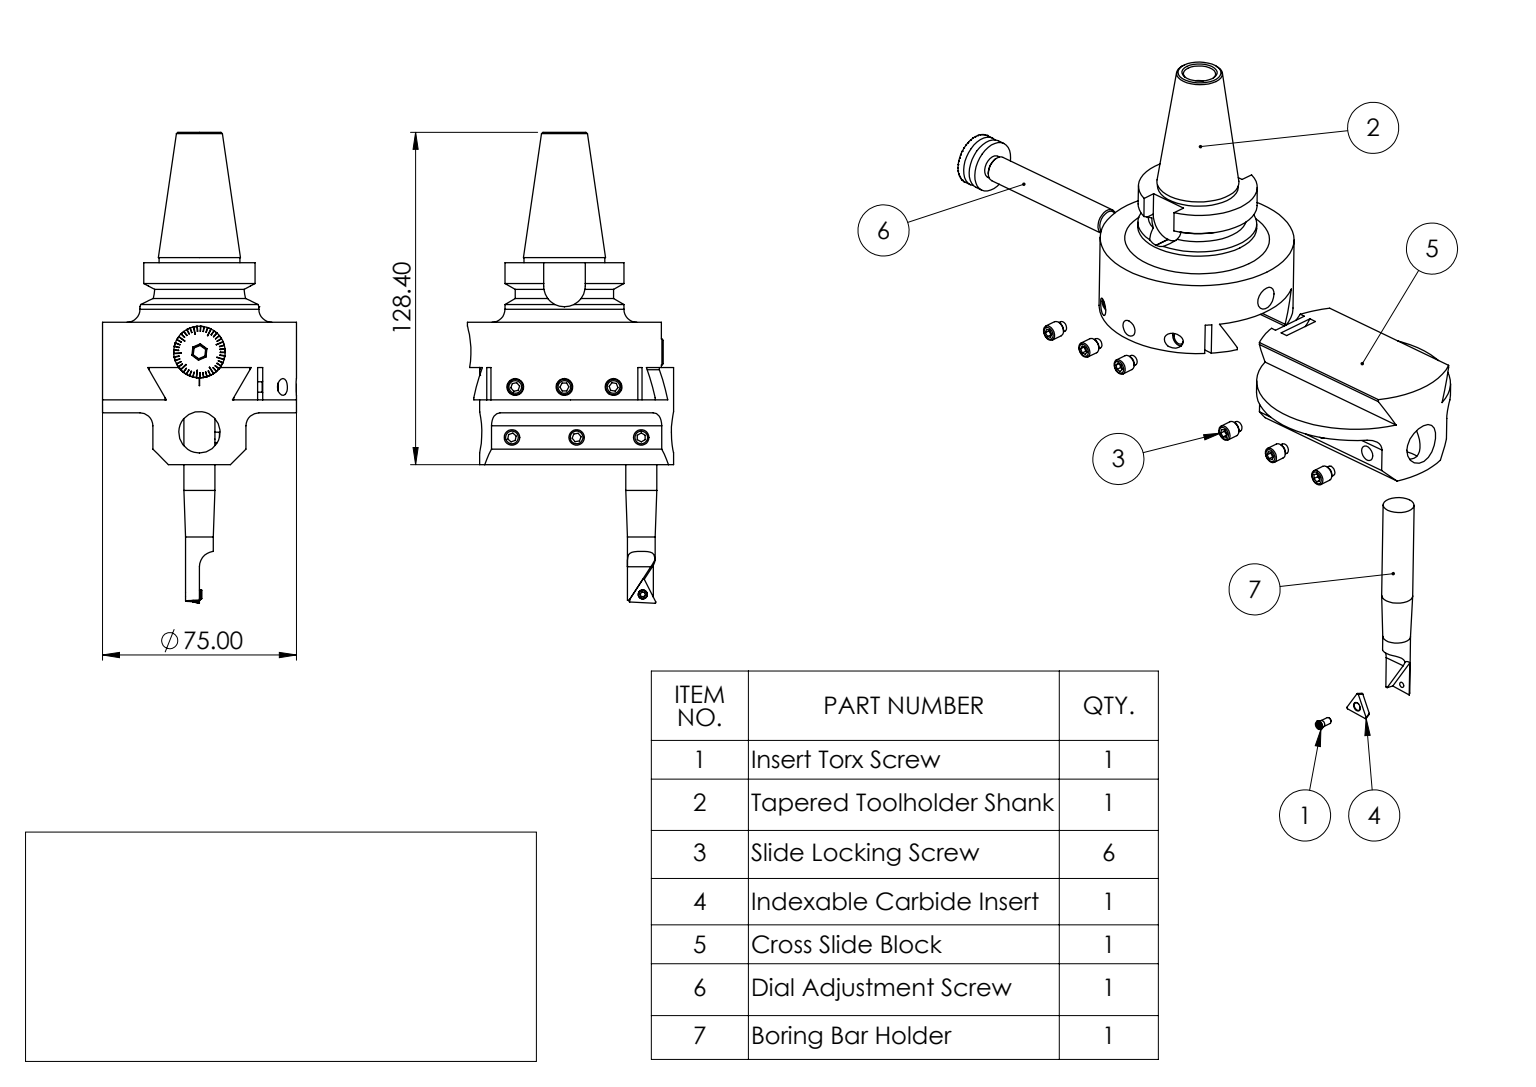
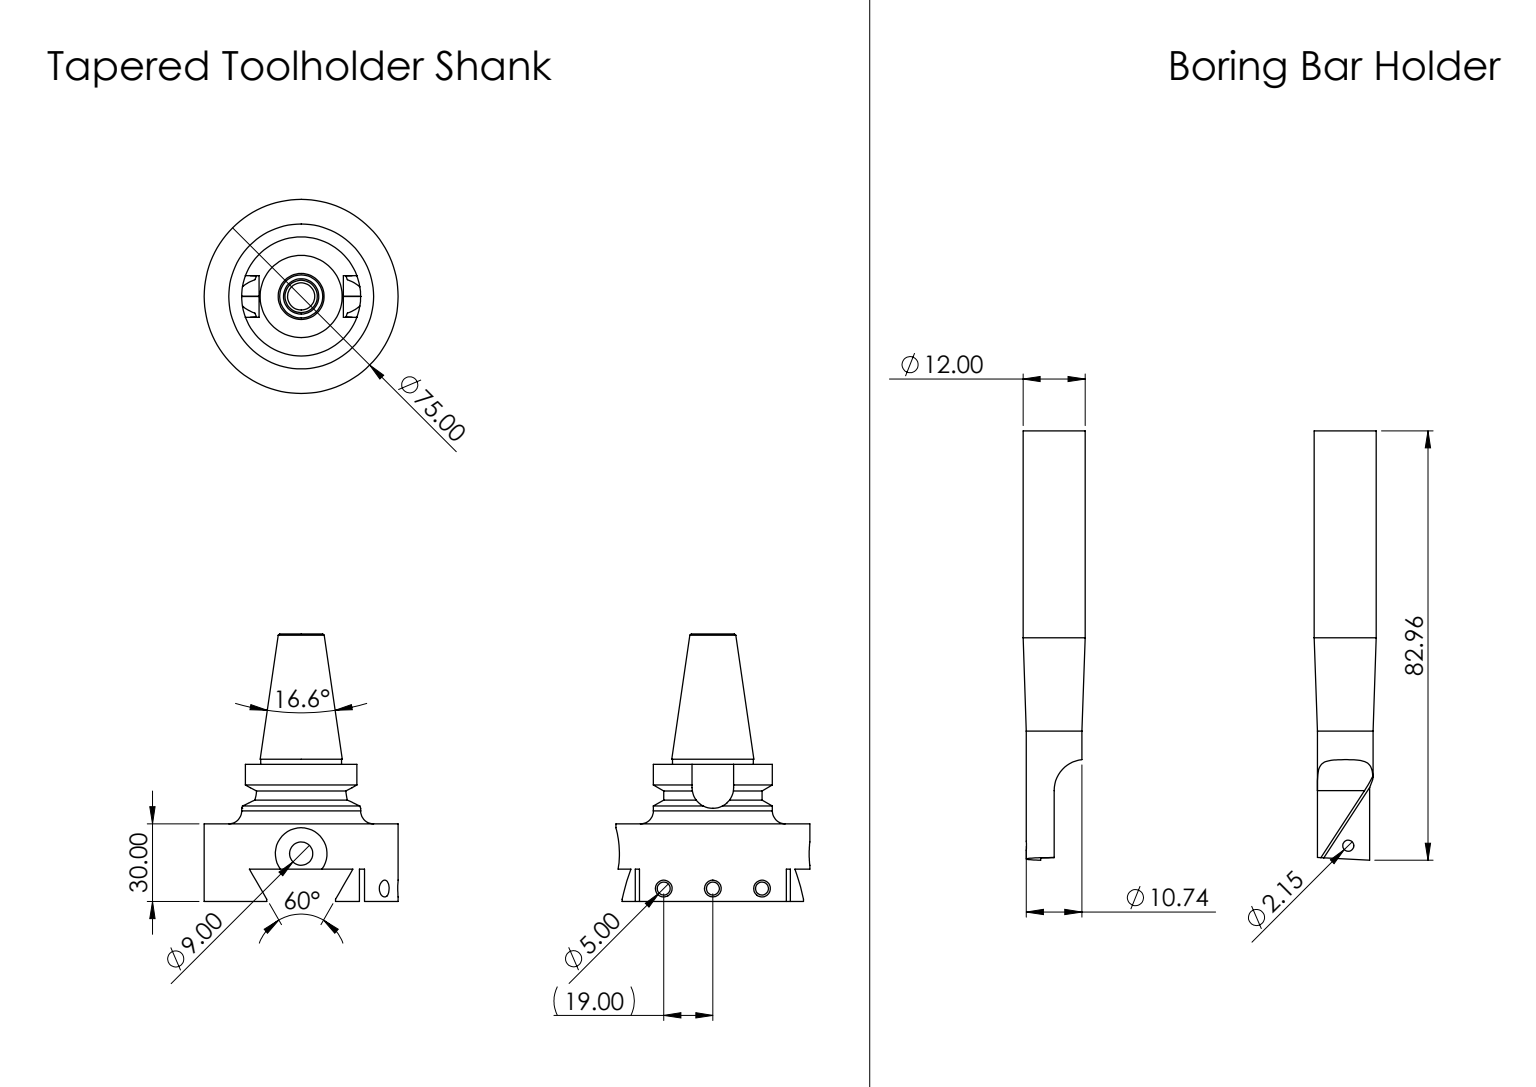
ISO-10303-21;
HEADER;
FILE_DESCRIPTION (('STEP AP214'),
    '1' );
FILE_NAME ('MAS-672',
    '2026-10-09T18:50:44',
    ( '' ),
    ( '' ),
    'SwSTEP 2.0',
    'SolidWorks 2026',
    '' );
FILE_SCHEMA (( 'AUTOMOTIVE_DESIGN' ));
ENDSEC;

DATA;
#1 = DIRECTION ( 'NONE',  ( 1.000000000000000000, 1.000000000000000078E-15, 0.000000000000000000 ) ) ;
#2 = ADVANCED_FACE ( 'NONE', ( #7489 ), #472, .F. ) ;
#3 = FACE_OUTER_BOUND ( 'NONE', #3774, .T. ) ;
#4 = EDGE_CURVE ( 'NONE', #9153, #8466, #14460, .T. ) ;
#5 =( BOUNDED_CURVE ( )  B_SPLINE_CURVE ( 3, ( #1335, #9589, #4703, #9365 ),
 .UNSPECIFIED., .F., .F. ) 
 B_SPLINE_CURVE_WITH_KNOTS ( ( 4, 4 ),
 ( 1.628044839356179940, 3.141592653589793116 ),
 .UNSPECIFIED. ) 
 CURVE ( )  GEOMETRIC_REPRESENTATION_ITEM ( )  RATIONAL_B_SPLINE_CURVE ( ( 1.000000000000000000, 0.8180365063541270576, 0.8180365063541270576, 1.000000000000000000 ) ) 
 REPRESENTATION_ITEM ( '' )  );
#6 = LINE ( 'NONE', #11551, #10906 ) ;
#7 = EDGE_CURVE ( 'NONE', #9450, #4202, #8492, .T. ) ;
#8 = LINE ( 'NONE', #14787, #7820 ) ;
#9 = CARTESIAN_POINT ( 'NONE',  ( -36.90121799483238618, -37.26927769664154511, 50.29562344872909563 ) ) ;
#10 = FACE_OUTER_BOUND ( 'NONE', #5268, .T. ) ;
#11 = ORIENTED_EDGE ( 'NONE', *, *, #1671, .F. ) ;
#12 = DIRECTION ( 'NONE',  ( 8.018662683283438208E-16, -5.975035461963189015E-16, -1.000000000000000000 ) ) ;
#13 = EDGE_LOOP ( 'NONE', ( #14568, #7332, #7097, #12565 ) ) ;
#15 = ORIENTED_EDGE ( 'NONE', *, *, #4138, .F. ) ;
#14 = CARTESIAN_POINT ( 'NONE',  ( -24.38380099443793725, -15.36048369738253427, 57.00231026484397745 ) ) ;
#16 = EDGE_CURVE ( 'NONE', #234, #9567, #717, .T. ) ;
#17 = VERTEX_POINT ( 'NONE', #8566 ) ;
#18 = AXIS2_PLACEMENT_3D ( 'NONE', #7899, #12589, #2105 ) ;
#19 = CYLINDRICAL_SURFACE ( 'NONE', #13148, 15.62500000000000000 ) ;
#20 = ORIENTED_EDGE ( 'NONE', *, *, #787, .F. ) ;
#21 = CYLINDRICAL_SURFACE ( 'NONE', #12948, 3.000000000000002665 ) ;
#22 = CARTESIAN_POINT ( 'NONE',  ( -15.49969986081095996, -67.00737899243799234, -5.497689735156000346 ) ) ;
#23 = CARTESIAN_POINT ( 'NONE',  ( 2.500300139188999182, -51.00737899243799944, -13.39525803434800011 ) ) ;
#24 = DIRECTION ( 'NONE',  ( 0.000000000000000000, 0.000000000000000000, 1.000000000000000000 ) ) ;
#25 = ADVANCED_FACE ( 'NONE', ( #12243 ), #13329, .T. ) ;
#26 = CARTESIAN_POINT ( 'NONE',  ( -19.99969986081099904, -13.50737899243800122, -13.01695671647154917 ) ) ;
#27 = CARTESIAN_POINT ( 'NONE',  ( -8.600581100527527667, -9.311215824554304632, 56.85231026484400019 ) ) ;
#28 = CARTESIAN_POINT ( 'NONE',  ( -21.52984724227062685, -49.79067269186487721, -17.51158402248789869 ) ) ;
#29 = ORIENTED_EDGE ( 'NONE', *, *, #1222, .T. ) ;
#30 = PLANE ( 'NONE',  #7847 ) ;
#31 = ORIENTED_EDGE ( 'NONE', *, *, #8737, .F. ) ;
#32 = DIRECTION ( 'NONE',  ( 0.4895147004624025855, -0.8719950447285834683, 9.135454576425998749E-16 ) ) ;
#33 = VERTEX_POINT ( 'NONE', #4056 ) ;
#34 = VERTEX_POINT ( 'NONE', #8713 ) ;
#35 = CARTESIAN_POINT ( 'NONE',  ( -10.39628701978575975, -6.002951807498697612, 56.85231026484398598 ) ) ;
#36 = VERTEX_POINT ( 'NONE', #13398 ) ;
#38 = EDGE_CURVE ( 'NONE', #4941, #11428, #1756, .T. ) ;
#37 = CARTESIAN_POINT ( 'NONE',  ( -15.57469986081333424, -23.50709773848279482, 57.00223526477140013 ) ) ;
#39 = CARTESIAN_POINT ( 'NONE',  ( -15.49969986081099904, 10.68321993080349763, 24.21206422150099868 ) ) ;
#40 = CARTESIAN_POINT ( 'NONE',  ( -10.66443468489866220, -90.61811337294874136, -7.838004541461820907 ) ) ;
#41 = CIRCLE ( 'NONE', #1011, 2.500000000000002220 ) ;
#42 = CARTESIAN_POINT ( 'NONE',  ( -7.506852801849951184, -44.86566843535796778, 21.38792573514972872 ) ) ;
#44 = CARTESIAN_POINT ( 'NONE',  ( -15.49969986081100615, -101.3912783891275069, -6.049618808461761255 ) ) ;
#43 = CARTESIAN_POINT ( 'NONE',  ( -15.50552586659557797, -13.55703840903364288, 56.85231026484398598 ) ) ;
#45 = ORIENTED_EDGE ( 'NONE', *, *, #9054, .F. ) ;
#46 = CARTESIAN_POINT ( 'NONE',  ( -15.17726793795939599, -10.75904990174046461, 51.00231026484399166 ) ) ;
#47 = CARTESIAN_POINT ( 'NONE',  ( -19.40475874296427250, -15.76281827183478512, -13.08441654828304657 ) ) ;
#48 = EDGE_LOOP ( 'NONE', ( #7800, #11011, #11564, #11938, #6650, #9579, #4015 ) ) ;
#49 = ORIENTED_EDGE ( 'NONE', *, *, #8035, .T. ) ;
#50 = CYLINDRICAL_SURFACE ( 'NONE', #2747, 15.62500000000000000 ) ;
#51 = FACE_BOUND ( 'NONE', #14476, .T. ) ;
#52 = ORIENTED_EDGE ( 'NONE', *, *, #5707, .T. ) ;
#53 = CARTESIAN_POINT ( 'NONE',  ( -10.22150846799388191, -38.48997916076172743, -17.62493476913342150 ) ) ;
#54 = EDGE_LOOP ( 'NONE', ( #11405, #3978, #7502, #8559 ) ) ;
#55 = EDGE_CURVE ( 'NONE', #11066, #9490, #2977, .T. ) ;
#56 = VECTOR ( 'NONE', #14424, 999.9999999999998863 ) ;
#57 = VECTOR ( 'NONE', #8652, 999.9999999999998863 ) ;
#58 = DIRECTION ( 'NONE',  ( -0.5104125104778984845, -0.8599296884906632021, 1.045284632676530333E-16 ) ) ;
#59 = CARTESIAN_POINT ( 'NONE',  ( -37.04494295528539993, 3.992621007561997892, 24.16206422150099442 ) ) ;
#60 = CARTESIAN_POINT ( 'NONE',  ( -15.49969986081091555, -109.7266455319748957, -5.512402352389309534 ) ) ;
#61 = CARTESIAN_POINT ( 'NONE',  ( -12.46042140754850713, -23.00808483377100444, 57.00231026484399166 ) ) ;
#62 = ORIENTED_EDGE ( 'NONE', *, *, #12874, .F. ) ;
#63 = DIRECTION ( 'NONE',  ( -0.3306575217771102193, 0.9437508163134058492, -8.290375725550400094E-16 ) ) ;
#64 = VECTOR ( 'NONE', #10695, 1000.000000000000000 ) ;
#65 = DIRECTION ( 'NONE',  ( 0.9354976265738682573, -0.3533329742249642913, 9.612616959383187437E-16 ) ) ;
#66 = ORIENTED_EDGE ( 'NONE', *, *, #12766, .T. ) ;
#67 = CIRCLE ( 'NONE', #8607, 9.974999999999999645 ) ;
#68 = AXIS2_PLACEMENT_3D ( 'NONE', #8168, #77, #12858 ) ;
#69 = CARTESIAN_POINT ( 'NONE',  ( -18.09969986081100402, -102.4362639876081289, -6.675878016713550522 ) ) ;
#70 = ORIENTED_EDGE ( 'NONE', *, *, #13189, .F. ) ;
#71 = DIRECTION ( 'NONE',  ( 0.000000000000000000, 0.000000000000000000, 1.000000000000000000 ) ) ;
#72 = EDGE_LOOP ( 'NONE', ( #9972, #5659, #4429, #2400 ) ) ;
#73 = EDGE_CURVE ( 'NONE', #9964, #7300, #12453, .T. ) ;
#74 = CARTESIAN_POINT ( 'NONE',  ( -5.499699860811000818, -46.50737899243799944, 22.50231026484399877 ) ) ;
#75 = DIRECTION ( 'NONE',  ( 1.000000000000000000, 0.000000000000000000, 0.000000000000000000 ) ) ;
#76 = ADVANCED_BREP_SHAPE_REPRESENTATION ( '', ( #2616, #6789 ), #5587 ) ;
#77 = DIRECTION ( 'NONE',  ( 0.7350174335289139105, -0.6780482080269579770, 9.945218953682734920E-16 ) ) ;
#78 = DIRECTION ( 'NONE',  ( 0.9931883319083343320, -0.1165201156931293391, 8.660254037844387408E-16 ) ) ;
#79 = AXIS2_PLACEMENT_3D ( 'NONE', #11806, #5987, #8360 ) ;
#80 = VECTOR ( 'NONE', #13700, 1000.000000000000114 ) ;
#81 = CARTESIAN_POINT ( 'NONE',  ( -15.49969986081099904, -32.00737899243799944, 24.21206422150100224 ) ) ;
#82 = FACE_OUTER_BOUND ( 'NONE', #1702, .T. ) ;
#83 = PLANE ( 'NONE',  #4186 ) ;
#84 = CARTESIAN_POINT ( 'NONE',  ( -7.424382730750140880, -13.52981220323889566, 56.85231026484400019 ) ) ;
#85 = ORIENTED_EDGE ( 'NONE', *, *, #97, .F. ) ;
#86 = CARTESIAN_POINT ( 'NONE',  ( -3.508527451664998686, -47.80641709811465745, -6.247689735156000346 ) ) ;
#87 = ORIENTED_EDGE ( 'NONE', *, *, #11967, .T. ) ;
#89 = EDGE_LOOP ( 'NONE', ( #13517, #1080, #433, #4734 ) ) ;
#88 = PLANE ( 'NONE',  #6660 ) ;
#90 = ORIENTED_EDGE ( 'NONE', *, *, #9916, .T. ) ;
#91 = CIRCLE ( 'NONE', #14500, 8.000000000000000000 ) ;
#92 = CIRCLE ( 'NONE', #3743, 3.249999999999999556 ) ;
#93 = EDGE_CURVE ( 'NONE', #6978, #3447, #6411, .T. ) ;
#94 = LINE ( 'NONE', #9566, #672 ) ;
#95 = ORIENTED_EDGE ( 'NONE', *, *, #10374, .T. ) ;
#96 = DIRECTION ( 'NONE',  ( -8.018662683283438208E-16, 5.975035461963189015E-16, 1.000000000000000000 ) ) ;
#97 = EDGE_CURVE ( 'NONE', #6821, #6890, #11166, .T. ) ;
#98 = CARTESIAN_POINT ( 'NONE',  ( -20.86490974387957209, -107.8289007898295182, -5.225852060212539563 ) ) ;
#99 =( BOUNDED_CURVE ( )  B_SPLINE_CURVE ( 3, ( #13212, #2486, #10670, #275 ),
 .UNSPECIFIED., .F., .T. ) 
 B_SPLINE_CURVE_WITH_KNOTS ( ( 4, 4 ),
 ( 4.712388980384689674, 6.283185307179586232 ),
 .UNSPECIFIED. ) 
 CURVE ( )  GEOMETRIC_REPRESENTATION_ITEM ( )  RATIONAL_B_SPLINE_CURVE ( ( 1.000000000000000000, 0.8047378541243649375, 0.8047378541243649375, 1.000000000000000000 ) ) 
 REPRESENTATION_ITEM ( '' )  );
#100 = LINE ( 'NONE', #14015, #4170 ) ;
#101 = CARTESIAN_POINT ( 'NONE',  ( 0.000000000000000000, 0.000000000000000000, 0.000000000000000000 ) ) ;
#102 = EDGE_CURVE ( 'NONE', #7782, #14676, #12670, .T. ) ;
#103 = DIRECTION ( 'NONE',  ( -0.9320450512859426162, -0.3618458327180910095, 0.01896353653557692268 ) ) ;
#104 = AXIS2_PLACEMENT_3D ( 'NONE', #5495, #8007, #12779 ) ;
#105 = CARTESIAN_POINT ( 'NONE',  ( -11.67714598312096008, -19.46131314156662384, 56.85231026484400019 ) ) ;
#106 = CARTESIAN_POINT ( 'NONE',  ( -5.499699860810999041, -13.50737899243800122, 6.712064221500998684 ) ) ;
#107 = APPLICATION_CONTEXT ( 'automotive_design' ) ;
#108 = ORIENTED_EDGE ( 'NONE', *, *, #1414, .F. ) ;
#109 = CARTESIAN_POINT ( 'NONE',  ( -14.90757383352018195, -17.97794807782672777, -13.28437183209255146 ) ) ;
#110 = ORIENTED_EDGE ( 'NONE', *, *, #5500, .T. ) ;
#111 = AXIS2_PLACEMENT_3D ( 'NONE', #10208, #14881, #11508 ) ;
#112 = ORIENTED_EDGE ( 'NONE', *, *, #3083, .T. ) ;
#113 = ORIENTED_EDGE ( 'NONE', *, *, #12612, .F. ) ;
#114 = CARTESIAN_POINT ( 'NONE',  ( -9.989347722329675605, -44.50737899243799944, -5.497689735156000346 ) ) ;
#115 = EDGE_CURVE ( 'NONE', #11608, #7250, #12699, .T. ) ;
#116 = CARTESIAN_POINT ( 'NONE',  ( 4.650967236384746073, -37.88568168827513460, 51.12989147907354948 ) ) ;
#117 = EDGE_CURVE ( 'NONE', #4448, #10428, #688, .T. ) ;
#118 = VERTEX_POINT ( 'NONE', #5499 ) ;
#119 = CARTESIAN_POINT ( 'NONE',  ( -15.49969986081092088, -13.50737899243822504, 57.00231026484397745 ) ) ;
#120 = LINE ( 'NONE', #11886, #1708 ) ;
#121 = CARTESIAN_POINT ( 'NONE',  ( -1.821162622431182765, -43.50737899243799234, -5.497689735156000346 ) ) ;
#122 = AXIS2_PLACEMENT_3D ( 'NONE', #7053, #14187, #10744 ) ;
#123 = LINE ( 'NONE', #4934, #14525 ) ;
#124 = COLOUR_RGB ( '', 0.72549020, 0.75294118, 0.79215686) ;
#126 = LINE ( 'NONE', #11658, #7291 ) ;
#125 = CARTESIAN_POINT ( 'NONE',  ( -7.500433020662222283, -49.00523987278725713, -5.609464624471996785 ) ) ;
#127 = ORIENTED_EDGE ( 'NONE', *, *, #115, .F. ) ;
#128 = DIRECTION ( 'NONE',  ( 0.000000000000000000, 0.000000000000000000, -1.000000000000000000 ) ) ;
#129 = DIRECTION ( 'NONE',  ( 0.9645173894937585368, 0.2640193276336892936, 6.156614753256587028E-16 ) ) ;
#130 = ORIENTED_EDGE ( 'NONE', *, *, #8611, .T. ) ;
#131 = CARTESIAN_POINT ( 'NONE',  ( -8.744347237509680681, -17.93190845158491342, 57.00231026484399166 ) ) ;
#132 = ADVANCED_FACE ( 'NONE', ( #4206 ), #14685, .F. ) ;
#133 = EDGE_LOOP ( 'NONE', ( #10977, #6757, #1819, #5580 ) ) ;
#134 = CARTESIAN_POINT ( 'NONE',  ( -3.508527451664998686, -47.37340439622244048, -6.997689735156000346 ) ) ;
#135 = ORIENTED_EDGE ( 'NONE', *, *, #11324, .F. ) ;
#136 = EDGE_CURVE ( 'NONE', #14079, #280, #5835, .T. ) ;
#137 = VECTOR ( 'NONE', #5946, 999.9999999999998863 ) ;
#138 = CARTESIAN_POINT ( 'NONE',  ( 7.500245791298697284, 3.992621007561997892, 24.26206422150100295 ) ) ;
#139 = DIRECTION ( 'NONE',  ( 0.000000000000000000, 0.1872998510044759646, 0.9823027872370621028 ) ) ;
#140 = ADVANCED_FACE ( 'NONE', ( #4434 ), #1914, .T. ) ;
#141 = DIRECTION ( 'NONE',  ( -8.018662683283438208E-16, 5.975035461963189015E-16, 1.000000000000000000 ) ) ;
#142 = CARTESIAN_POINT ( 'NONE',  ( 18.53245405280430802, -27.00737899243800300, 8.462064221501000461 ) ) ;
#143 = ORIENTED_EDGE ( 'NONE', *, *, #1430, .T. ) ;
#144 = FACE_OUTER_BOUND ( 'NONE', #9192, .T. ) ;
#145 = DIRECTION ( 'NONE',  ( 8.660254037844386422E-16, -0.8660254037844387076, -0.4999999999999998890 ) ) ;
#146 = ORIENTED_EDGE ( 'NONE', *, *, #10088, .T. ) ;
#147 = DIRECTION ( 'NONE',  ( -1.000000000000000000, 1.499759782661860071E-32, -1.224646799147350002E-16 ) ) ;
#148 = EDGE_LOOP ( 'NONE', ( #12283, #12107, #2323, #5497, #12543, #7117, #9032, #3787, #13140, #10913, #13822, #11755, #4698, #10634, #4086, #13650, #1565 ) ) ;
#149 = PLANE ( 'NONE',  #14987 ) ;
#150 = VERTEX_POINT ( 'NONE', #916 ) ;
#151 = CARTESIAN_POINT ( 'NONE',  ( 2.500300139188999182, -51.00737899243799944, -13.39525803434800011 ) ) ;
#152 = CARTESIAN_POINT ( 'NONE',  ( -1.821162622431182765, -43.50737899243799234, -5.497689735156000346 ) ) ;
#153 = CARTESIAN_POINT ( 'NONE',  ( -28.28282149594069850, -32.00737899243799944, -17.99768973515599768 ) ) ;
#154 = FACE_OUTER_BOUND ( 'NONE', #467, .T. ) ;
#155 = DIRECTION ( 'NONE',  ( 0.000000000000000000, 0.000000000000000000, 1.000000000000000000 ) ) ;
#156 = CARTESIAN_POINT ( 'NONE',  ( -17.71860670988920816, -11.85398021090886367, 51.00231026484399166 ) ) ;
#157 = VECTOR ( 'NONE', #7597, 1000.000000000000114 ) ;
#158 = VECTOR ( 'NONE', #4649, 1000.000000000000000 ) ;
#159 = EDGE_CURVE ( 'NONE', #10747, #3108, #3053, .T. ) ;
#160 = CARTESIAN_POINT ( 'NONE',  ( -20.87112600995946110, -106.2635794615412834, -5.497689735156005675 ) ) ;
#161 = ORIENTED_EDGE ( 'NONE', *, *, #9054, .T. ) ;
#162 = LINE ( 'NONE', #9710, #2630 ) ;
#163 = CARTESIAN_POINT ( 'NONE',  ( -37.26807582031575805, -37.15669500878452425, 50.03818627108570638 ) ) ;
#164 = DIRECTION ( 'NONE',  ( 0.000000000000000000, 1.131341397376178572E-16, -1.000000000000000000 ) ) ;
#165 = ORIENTED_EDGE ( 'NONE', *, *, #2149, .T. ) ;
#166 = DIRECTION ( 'NONE',  ( 8.018662683283438208E-16, -5.975035461963189015E-16, -1.000000000000000000 ) ) ;
#167 = ORIENTED_EDGE ( 'NONE', *, *, #12641, .F. ) ;
#169 = ORIENTED_EDGE ( 'NONE', *, *, #13036, .F. ) ;
#168 = FACE_BOUND ( 'NONE', #682, .T. ) ;
#170 = ORIENTED_EDGE ( 'NONE', *, *, #333, .F. ) ;
#171 = CARTESIAN_POINT ( 'NONE',  ( -15.49969986081092088, -13.50737899243822504, 56.85231026484398598 ) ) ;
#172 = ORIENTED_EDGE ( 'NONE', *, *, #3900, .F. ) ;
#173 = FACE_OUTER_BOUND ( 'NONE', #4854, .T. ) ;
#174 = CARTESIAN_POINT ( 'NONE',  ( -15.49969986081099904, -44.50737899243799944, -109.5506571639849938 ) ) ;
#175 = SHAPE_REPRESENTATION_RELATIONSHIP ( 'NONE' , 'NONE' ,  #13495, #6601 ) ;
#176 = CARTESIAN_POINT ( 'NONE',  ( -18.41596830400278506, -14.76384693893611910, 57.00231026484397745 ) ) ;
#177 = EDGE_CURVE ( 'NONE', #13055, #12587, #8525, .T. ) ;
#178 = AXIS2_PLACEMENT_3D ( 'NONE', #14596, #7550, #6095 ) ;
#179 = CARTESIAN_POINT ( 'NONE',  ( -15.49969986081099371, -9.007378992438001220, -13.28793577849899599 ) ) ;
#180 = CARTESIAN_POINT ( 'NONE',  ( -28.78282149594069850, -32.00737899243799944, 24.21206422150099868 ) ) ;
#181 = EDGE_CURVE ( 'NONE', #13469, #7197, #14834, .T. ) ;
#182 = CARTESIAN_POINT ( 'NONE',  ( 4.224496369445544630, -38.22985747236960918, -12.39136299437819488 ) ) ;
#183 = EDGE_LOOP ( 'NONE', ( #8383, #10689, #169, #12159 ) ) ;
#184 = ORIENTED_EDGE ( 'NONE', *, *, #9513, .F. ) ;
#185 = AXIS2_PLACEMENT_3D ( 'NONE', #4466, #10423, #5753 ) ;
#186 = VERTEX_POINT ( 'NONE', #14912 ) ;
#187 = CARTESIAN_POINT ( 'NONE',  ( 2.883830742001312508, -40.08477038827061989, 52.18712618527332125 ) ) ;
#188 = ORIENTED_EDGE ( 'NONE', *, *, #5314, .T. ) ;
#189 = CIRCLE ( 'NONE', #12147, 2.499999999999999556 ) ;
#190 = DIRECTION ( 'NONE',  ( 1.000000000000000000, 1.000000000000000078E-15, 1.000000000000000078E-15 ) ) ;
#191 = FACE_OUTER_BOUND ( 'NONE', #10169, .T. ) ;
#192 = DIRECTION ( 'NONE',  ( 0.5975035461963189576, 0.8018662683283437342, 0.000000000000000000 ) ) ;
#193 = EDGE_CURVE ( 'NONE', #1606, #4275, #8746, .T. ) ;
#194 = EDGE_CURVE ( 'NONE', #4315, #8561, #7264, .T. ) ;
#195 = CARTESIAN_POINT ( 'NONE',  ( -15.49969986081091022, -13.50737899243823215, 46.00231026484398456 ) ) ;
#197 = CARTESIAN_POINT ( 'NONE',  ( -8.681233859935401753, -6.226640953275941470, 56.85231026484398598 ) ) ;
#196 = LINE ( 'NONE', #3708, #2723 ) ;
#198 = EDGE_CURVE ( 'NONE', #14370, #12333, #7164, .T. ) ;
#199 = EDGE_LOOP ( 'NONE', ( #11824, #6464, #11368, #3598 ) ) ;
#200 = CARTESIAN_POINT ( 'NONE',  ( -15.49969986081099904, -19.50737899243800300, 24.21206422150100224 ) ) ;
#201 = AXIS2_PLACEMENT_3D ( 'NONE', #9207, #12513, #13890 ) ;
#202 = CARTESIAN_POINT ( 'NONE',  ( -7.499699860810999041, -19.50737899243799589, 51.00231026484400587 ) ) ;
#203 = EDGE_LOOP ( 'NONE', ( #1328, #2305, #6910, #14868 ) ) ;
#204 = ORIENTED_EDGE ( 'NONE', *, *, #10815, .T. ) ;
#205 = AXIS2_PLACEMENT_3D ( 'NONE', #2653, #1576, #13144 ) ;
#206 = CARTESIAN_POINT ( 'NONE',  ( -16.55248250669792753, -52.45523696625489407, 56.99108552064786437 ) ) ;
#207 = ORIENTED_EDGE ( 'NONE', *, *, #11956, .F. ) ;
#208 =( NAMED_UNIT ( * ) SI_UNIT ( $, .STERADIAN. ) SOLID_ANGLE_UNIT ( ) );
#209 = CARTESIAN_POINT ( 'NONE',  ( 7.464989229556169725, 4.086072560925113173, 25.52420958079008884 ) ) ;
#210 = CARTESIAN_POINT ( 'NONE',  ( -17.47506273705024071, -21.33739760717825718, 56.85231026484400019 ) ) ;
#211 = EDGE_CURVE ( 'NONE', #12427, #2827, #11544, .T. ) ;
#212 = DIRECTION ( 'NONE',  ( 0.6859287159822015090, -0.7276687409742212953, 9.848077530122081084E-16 ) ) ;
#213 = CARTESIAN_POINT ( 'NONE',  ( -15.49969986081099016, -52.50737899243799944, 27.50231026484399521 ) ) ;
#214 = EDGE_CURVE ( 'NONE', #2810, #1679, #14130, .T. ) ;
#215 = ORIENTED_EDGE ( 'NONE', *, *, #13065, .F. ) ;
#216 = DIRECTION ( 'NONE',  ( 0.000000000000000000, 0.000000000000000000, 1.000000000000000000 ) ) ;
#217 = CARTESIAN_POINT ( 'NONE',  ( -10.84210729886283531, -6.910555398701176522, 56.85231026484398598 ) ) ;
#218 = ORIENTED_EDGE ( 'NONE', *, *, #1842, .T. ) ;
#219 = PLANE ( 'NONE',  #12030 ) ;
#220 = CARTESIAN_POINT ( 'NONE',  ( -15.49969986081099904, 0.9926210075619987805, 24.21206422150099868 ) ) ;
#221 = VERTEX_POINT ( 'NONE', #11762 ) ;
#222 = VECTOR ( 'NONE', #14585, 1000.000000000000000 ) ;
#223 = DIRECTION ( 'NONE',  ( -1.000000000000000000, -1.201369187114119994E-15, -9.616040805000176517E-16 ) ) ;
#224 = ORIENTED_EDGE ( 'NONE', *, *, #12134, .T. ) ;
#225 = FACE_OUTER_BOUND ( 'NONE', #3388, .T. ) ;
#226 = CARTESIAN_POINT ( 'NONE',  ( -15.49969986081098838, -17.75737899243799944, 48.00231026484399877 ) ) ;
#227 = EDGE_CURVE ( 'NONE', #9086, #8293, #11691, .T. ) ;
#228 = LINE ( 'NONE', #8628, #3240 ) ;
#230 = VECTOR ( 'NONE', #6999, 1000.000000000000000 ) ;
#229 = CARTESIAN_POINT ( 'NONE',  ( -7.753733168396170328, -46.50737899243799944, 47.00231026484399877 ) ) ;
#231 = AXIS2_PLACEMENT_3D ( 'NONE', #5849, #3193, #3340 ) ;
#232 = PLANE ( 'NONE',  #13853 ) ;
#233 = DIRECTION ( 'NONE',  ( 0.000000000000000000, 0.000000000000000000, 1.000000000000000000 ) ) ;
#234 = VERTEX_POINT ( 'NONE', #10472 ) ;
#235 = DIRECTION ( 'NONE',  ( -8.018662683283438208E-16, 5.975035461963189015E-16, 1.000000000000000000 ) ) ;
#236 = CARTESIAN_POINT ( 'NONE',  ( -16.32407967933980686, -20.53418644068968746, 57.00231026484399166 ) ) ;
#237 = CARTESIAN_POINT ( 'NONE',  ( -15.49969986081099727, -52.50737899243799944, 2.502310264843994769 ) ) ;
#238 = ORIENTED_EDGE ( 'NONE', *, *, #5431, .T. ) ;
#239 = DIRECTION ( 'NONE',  ( 8.018662683283438208E-16, -5.975035461963189015E-16, -1.000000000000000000 ) ) ;
#240 = VECTOR ( 'NONE', #12413, 1000.000000000000000 ) ;
#241 = ORIENTED_EDGE ( 'NONE', *, *, #492, .T. ) ;
#243 = ORIENTED_EDGE ( 'NONE', *, *, #13545, .T. ) ;
#242 = CARTESIAN_POINT ( 'NONE',  ( -18.04596724311489808, -11.61005040962811563, 57.00231026484397745 ) ) ;
#244 = ORIENTED_EDGE ( 'NONE', *, *, #12022, .T. ) ;
#245 = AXIS2_PLACEMENT_3D ( 'NONE', #11135, #508, #11280 ) ;
#246 = DIRECTION ( 'NONE',  ( 0.6626200482157384997, -0.03919731383111437623, -0.7479293030032968526 ) ) ;
#247 = ORIENTED_EDGE ( 'NONE', *, *, #4682, .F. ) ;
#248 = EDGE_CURVE ( 'NONE', #9045, #3429, #2887, .T. ) ;
#249 = PLANE ( 'NONE',  #11119 ) ;
#250 = CYLINDRICAL_SURFACE ( 'NONE', #2706, 6.000000000000000000 ) ;
#251 = CARTESIAN_POINT ( 'NONE',  ( 4.510281037539698445E-14, -66.39050128843828702, 86.90304541097793845 ) ) ;
#252 = DIRECTION ( 'NONE',  ( 0.5975035461963189576, 0.8018662683283437342, 0.000000000000000000 ) ) ;
#253 = CIRCLE ( 'NONE', #14173, 37.50000000000000000 ) ;
#254 = CARTESIAN_POINT ( 'NONE',  ( -24.01584079503567182, -10.37104457333969876, 57.00231026484397745 ) ) ;
#255 = CARTESIAN_POINT ( 'NONE',  ( -15.47224238247604511, -13.54916519690201149, 56.85231026484398598 ) ) ;
#256 = VECTOR ( 'NONE', #11415, 1000.000000000000114 ) ;
#257 = ORIENTED_EDGE ( 'NONE', *, *, #6613, .T. ) ;
#258 = SURFACE_SIDE_STYLE ('',( #7350 ) ) ;
#259 = VERTEX_POINT ( 'NONE', #1213 ) ;
#260 = ORIENTED_EDGE ( 'NONE', *, *, #6343, .T. ) ;
#261 = CARTESIAN_POINT ( 'NONE',  ( 5.515696375138871232, -37.41693849659856141, 50.56059116161328859 ) ) ;
#262 = ORIENTED_EDGE ( 'NONE', *, *, #3647, .F. ) ;
#263 = CARTESIAN_POINT ( 'NONE',  ( -23.39388780995641781, -11.80648316271623877, 56.85231026484398598 ) ) ;
#264 = PRODUCT ( 'Boring Bar Holder', 'Boring Bar Holder', '', ( #2047 ) ) ;
#265 = DIRECTION ( 'NONE',  ( 0.000000000000000000, 0.000000000000000000, 1.000000000000000000 ) ) ;
#266 = EDGE_CURVE ( 'NONE', #5839, #14925, #4584, .T. ) ;
#267 = EDGE_CURVE ( 'NONE', #7737, #2967, #4813, .T. ) ;
#268 = DIRECTION ( 'NONE',  ( 0.000000000000000000, 1.224646799147350002E-16, -1.000000000000000000 ) ) ;
#269 = CARTESIAN_POINT ( 'NONE',  ( -11.86438417805047862, -90.99861266563027584, -9.452020815084084759 ) ) ;
#270 = CIRCLE ( 'NONE', #3683, 9.974999999999999645 ) ;
#271 = DIRECTION ( 'NONE',  ( 1.000000000000000000, -3.922012711866029438E-32, 3.202566417187950042E-16 ) ) ;
#273 = CARTESIAN_POINT ( 'NONE',  ( -34.99969986081099904, -19.50737899243800300, 51.53354502093799994 ) ) ;
#272 = CARTESIAN_POINT ( 'NONE',  ( -7.749729581313432369, -48.02091033734640035, -3.487279356396127739 ) ) ;
#274 = EDGE_LOOP ( 'NONE', ( #8027, #11892 ) ) ;
#275 = CARTESIAN_POINT ( 'NONE',  ( -15.49969986081099727, -36.50737899243799944, 2.502310264843996546 ) ) ;
#276 = VERTEX_POINT ( 'NONE', #1064 ) ;
#277 = ORIENTED_EDGE ( 'NONE', *, *, #6216, .F. ) ;
#278 = CARTESIAN_POINT ( 'NONE',  ( 21.96528021387864271, -29.82714745920393185, 22.58218370277269571 ) ) ;
#279 = CARTESIAN_POINT ( 'NONE',  ( -5.499699860811003482, -46.50737899243799944, 44.50231026484399877 ) ) ;
#280 = VERTEX_POINT ( 'NONE', #11617 ) ;
#281 = CARTESIAN_POINT ( 'NONE',  ( -14.45170227088251202, -36.55910949265851428, -17.98655532003696678 ) ) ;
#282 = EDGE_CURVE ( 'NONE', #626, #3416, #13005, .T. ) ;
#283 = EDGE_CURVE ( 'NONE', #10750, #11940, #6056, .T. ) ;
#284 = ADVANCED_FACE ( 'NONE', ( #2513 ), #11846, .F. ) ;
#285 = DIRECTION ( 'NONE',  ( 0.000000000000000000, 0.000000000000000000, -1.000000000000000000 ) ) ;
#286 = AXIS2_PLACEMENT_3D ( 'NONE', #4236, #8813, #2856 ) ;
#287 = CARTESIAN_POINT ( 'NONE',  ( -15.49969986081099904, -32.00737899243799944, 24.21206422150100224 ) ) ;
#288 = EDGE_CURVE ( 'NONE', #14042, #11463, #13916, .T. ) ;
#289 = CARTESIAN_POINT ( 'NONE',  ( -24.32830346761242879, -18.15026423267100597, 56.85231026484398598 ) ) ;
#290 = PLANE ( 'NONE',  #9367 ) ;
#291 = ORIENTED_EDGE ( 'NONE', *, *, #2351, .F. ) ;
#292 = CARTESIAN_POINT ( 'NONE',  ( 4.500300139189000959, -19.50737899243801010, 55.93350807262470425 ) ) ;
#293 = CARTESIAN_POINT ( 'NONE',  ( 0.8003001391889992266, 11.99262100756199878, 24.26206422150100295 ) ) ;
#294 = ORIENTED_EDGE ( 'NONE', *, *, #11168, .F. ) ;
#295 = DIRECTION ( 'NONE',  ( 0.9437508163134050720, 0.3306575217771122732, 5.591929034707472732E-16 ) ) ;
#296 = DIRECTION ( 'NONE',  ( 0.000000000000000000, 1.000000000000000000, 1.224646799147350002E-16 ) ) ;
#297 = ORIENTED_EDGE ( 'NONE', *, *, #1602, .F. ) ;
#298 = LINE ( 'NONE', #4183, #349 ) ;
#299 = ORIENTED_EDGE ( 'NONE', *, *, #12335, .F. ) ;
#300 = DIRECTION ( 'NONE',  ( 1.000000000000000000, 1.201369187114119994E-15, 9.616040805000176517E-16 ) ) ;
#301 = VECTOR ( 'NONE', #1890, 1000.000000000000000 ) ;
#302 = EDGE_CURVE ( 'NONE', #14153, #6582, #13638, .T. ) ;
#303 = EDGE_CURVE ( 'NONE', #11878, #6778, #8167, .T. ) ;
#304 = CARTESIAN_POINT ( 'NONE',  ( -15.49969986081100437, -101.4268716156739600, -6.728778029351857981 ) ) ;
#305 = DIRECTION ( 'NONE',  ( -8.673617379884027583E-16, 1.000000000000000000, 0.000000000000000000 ) ) ;
#306 = DIRECTION ( 'NONE',  ( 0.2301973227387160703, -0.9731439732146149879, 7.660444431189776467E-16 ) ) ;
#307 = VECTOR ( 'NONE', #2927, 999.9999999999998863 ) ;
#308 = CIRCLE ( 'NONE', #8106, 9.974999999999999645 ) ;
#309 = VECTOR ( 'NONE', #4436, 1000.000000000000000 ) ;
#310 = LINE ( 'NONE', #9632, #1371 ) ;
#311 = ORIENTED_EDGE ( 'NONE', *, *, #9034, .F. ) ;
#312 = DIRECTION ( 'NONE',  ( 1.000000000000000000, -3.922012711866029438E-32, 3.202566417187950042E-16 ) ) ;
#313 = DIRECTION ( 'NONE',  ( 1.000000000000000000, 1.201369187114119994E-15, 9.616040805000176517E-16 ) ) ;
#314 = ADVANCED_FACE ( 'NONE', ( #7004, #5865, #10542, #6834 ), #10286, .F. ) ;
#315 = CARTESIAN_POINT ( 'NONE',  ( -23.54151295824578227, -12.77219731018227300, 57.00231026484397745 ) ) ;
#316 = CARTESIAN_POINT ( 'NONE',  ( -6.938526287600617515, -8.388108336439909607, 57.00231026484399166 ) ) ;
#318 = ORIENTED_EDGE ( 'NONE', *, *, #7751, .T. ) ;
#317 = CARTESIAN_POINT ( 'NONE',  ( -14.61203582816999891, -107.9994814593942607, -7.057848339359947154 ) ) ;
#319 = ORIENTED_EDGE ( 'NONE', *, *, #11952, .F. ) ;
#320 = DIRECTION ( 'NONE',  ( -0.1855175943453192255, -0.9826409426582660700, 4.383711467890751032E-16 ) ) ;
#321 = FACE_OUTER_BOUND ( 'NONE', #7198, .T. ) ;
#322 = EDGE_LOOP ( 'NONE', ( #14404, #10872, #12403, #8371 ) ) ;
#323 = VECTOR ( 'NONE', #13122, 1000.000000000000114 ) ;
#324 =( BOUNDED_CURVE ( )  B_SPLINE_CURVE ( 3, ( #292, #8307, #2730, #6008 ),
 .UNSPECIFIED., .F., .T. ) 
 B_SPLINE_CURVE_WITH_KNOTS ( ( 4, 4 ),
 ( 1.008260082251040135, 1.208720131788790120 ),
 .UNSPECIFIED. ) 
 CURVE ( )  GEOMETRIC_REPRESENTATION_ITEM ( )  RATIONAL_B_SPLINE_CURVE ( ( 1.000000000000000000, 0.9966541165307394312, 0.9966541165307394312, 1.000000000000000000 ) ) 
 REPRESENTATION_ITEM ( '' )  );
#325 = DIRECTION ( 'NONE',  ( 0.9988970074402866439, -0.04695496274985035134, 8.290375725550441510E-16 ) ) ;
#326 = VECTOR ( 'NONE', #4845, 1000.000000000000000 ) ;
#327 = ADVANCED_FACE ( 'NONE', ( #7907 ), #7823, .T. ) ;
#328 = PLANE ( 'NONE',  #5014 ) ;
#329 = DIRECTION ( 'NONE',  ( -8.018662683283438208E-16, 5.975035461963189015E-16, 1.000000000000000000 ) ) ;
#330 = CARTESIAN_POINT ( 'NONE',  ( 0.000000000000000000, 0.000000000000000000, 0.000000000000000000 ) ) ;
#331 = CARTESIAN_POINT ( 'NONE',  ( -16.66466864975539153, -9.150908980254410352, -13.27094003038157943 ) ) ;
#332 = B_SPLINE_CURVE_WITH_KNOTS ( 'NONE', 3,
 ( #3786, #14269, #2413, #7056, #11734, #2637, #7211, #5838 ),
 .UNSPECIFIED., .F., .F.,
 ( 4, 2, 2, 4 ),
 ( 0.000000000000000000, 0.2500000000000007216, 0.5000000000000014433, 1.000000000000000000 ),
 .UNSPECIFIED. ) ;
#333 = EDGE_CURVE ( 'NONE', #11915, #14532, #10956, .T. ) ;
#334 = EDGE_CURVE ( 'NONE', #9332, #3237, #5095, .T. ) ;
#335 = AXIS2_PLACEMENT_3D ( 'NONE', #317, #9563, #3755 ) ;
#336 = DIRECTION ( 'NONE',  ( 8.018662683283438208E-16, -5.975035461963189015E-16, -1.000000000000000000 ) ) ;
#337 = VERTEX_POINT ( 'NONE', #13812 ) ;
#338 = CARTESIAN_POINT ( 'NONE',  ( -15.49969986081099904, -57.00737899243801365, 57.00231026484399166 ) ) ;
#339 = CONICAL_SURFACE ( 'NONE', #2284, 1664.279482350500075, 1.029744258676650093 ) ;
#340 = ORIENTED_EDGE ( 'NONE', *, *, #454, .F. ) ;
#341 = LINE ( 'NONE', #7503, #3156 ) ;
#342 = DIRECTION ( 'NONE',  ( -1.169602638241521591E-15, 0.1872998510044552312, 0.9823027872370662106 ) ) ;
#343 = ORIENTED_EDGE ( 'NONE', *, *, #4783, .T. ) ;
#344 = ORIENTED_EDGE ( 'NONE', *, *, #5377, .F. ) ;
#345 = CARTESIAN_POINT ( 'NONE',  ( -15.49969986081099904, -32.00737899243799944, 24.21206422150100224 ) ) ;
#346 = ORIENTED_EDGE ( 'NONE', *, *, #6966, .T. ) ;
#347 = LINE ( 'NONE', #11884, #5404 ) ;
#348 = DIRECTION ( 'NONE',  ( 8.018662683283438208E-16, -5.975035461963189015E-16, -1.000000000000000000 ) ) ;
#349 = VECTOR ( 'NONE', #8838, 1000.000000000000114 ) ;
#350 = FILL_AREA_STYLE ('',( #10818 ) ) ;
#351 = CARTESIAN_POINT ( 'NONE',  ( -16.26465502354534465, -4.464365468230401923, 56.85231026484398598 ) ) ;
#352 = CONICAL_SURFACE ( 'NONE', #10852, 6.000000000000001776, 0.03490658503988566114 ) ;
#353 = CARTESIAN_POINT ( 'NONE',  ( -15.49969986081091022, -13.50737899243823215, 45.50231026484398456 ) ) ;
#354 = EDGE_CURVE ( 'NONE', #745, #9450, #1038, .T. ) ;
#356 = CARTESIAN_POINT ( 'NONE',  ( -15.61203582816999891, -108.2036686363109084, -6.241690937583108223 ) ) ;
#355 = CARTESIAN_POINT ( 'NONE',  ( -20.31707134655588121, -4.772760685475329723, 57.00231026484397745 ) ) ;
#357 = ORIENTED_EDGE ( 'NONE', *, *, #4575, .F. ) ;
#358 = CARTESIAN_POINT ( 'NONE',  ( -17.98267069058175593, -13.21607870320540279, 51.25231026484399166 ) ) ;
#359 = CARTESIAN_POINT ( 'NONE',  ( -14.15531688186919901, -11.70317988869945580, 51.25231026484399166 ) ) ;
#360 = ORIENTED_EDGE ( 'NONE', *, *, #12281, .T. ) ;
#361 = ORIENTED_EDGE ( 'NONE', *, *, #5740, .T. ) ;
#362 = VECTOR ( 'NONE', #6575, 1000.000000000000000 ) ;
#363 = CARTESIAN_POINT ( 'NONE',  ( -19.50440554761897261, -37.57692853466172522, 56.78858631758297548 ) ) ;
#364 = VERTEX_POINT ( 'NONE', #963 ) ;
#365 = CARTESIAN_POINT ( 'NONE',  ( 2.374542637206501272, 7.183219930803497633, 17.76912582958182085 ) ) ;
#366 = AXIS2_PLACEMENT_3D ( 'NONE', #8590, #7864, #7944 ) ;
#367 = CARTESIAN_POINT ( 'NONE',  ( 7.367243934124074300, 4.365428709207489710, 26.75804073331549304 ) ) ;
#368 = VECTOR ( 'NONE', #4802, 1000.000000000000000 ) ;
#369 = LINE ( 'NONE', #7224, #14846 ) ;
#370 = UNCERTAINTY_MEASURE_WITH_UNIT (LENGTH_MEASURE( 1.000000000000000082E-05 ), #958, 'distance_accuracy_value', 'NONE');
#371 = CARTESIAN_POINT ( 'NONE',  ( -9.204203523554131294, -8.449911655164932256, 56.85231026484398598 ) ) ;
#372 = EDGE_CURVE ( 'NONE', #4377, #1107, #9059, .T. ) ;
#373 = DIRECTION ( 'NONE',  ( -8.018662683283438208E-16, 5.975035461963189015E-16, 1.000000000000000000 ) ) ;
#374 = VERTEX_POINT ( 'NONE', #1959 ) ;
#375 = LINE ( 'NONE', #5935, #15083 ) ;
#376 = DIRECTION ( 'NONE',  ( 0.000000000000000000, 0.000000000000000000, 1.000000000000000000 ) ) ;
#377 = EDGE_LOOP ( 'NONE', ( #6122, #12748, #11270, #7433 ) ) ;
#378 = EDGE_CURVE ( 'NONE', #12795, #6835, #5541, .T. ) ;
#379 = PLANE ( 'NONE',  #13903 ) ;
#380 = PRESENTATION_STYLE_ASSIGNMENT (( #3958 ) ) ;
#381 = EDGE_LOOP ( 'NONE', ( #709, #10098 ) ) ;
#382 = LINE ( 'NONE', #13374, #828 ) ;
#383 = EDGE_LOOP ( 'NONE', ( #11482, #7292, #5223, #897 ) ) ;
#384 = DIRECTION ( 'NONE',  ( 0.000000000000000000, -1.000000000000000000, -1.224646799147350002E-16 ) ) ;
#385 = DIRECTION ( 'NONE',  ( -1.000000000000000000, 0.000000000000000000, 0.000000000000000000 ) ) ;
#386 = CARTESIAN_POINT ( 'NONE',  ( -7.813858722443232097, -47.64803766822201680, 17.27706589258430014 ) ) ;
#387 = LINE ( 'NONE', #9553, #4308 ) ;
#388 = EDGE_CURVE ( 'NONE', #12884, #3001, #2110, .T. ) ;
#389 = ORIENTED_EDGE ( 'NONE', *, *, #14266, .F. ) ;
#390 = CARTESIAN_POINT ( 'NONE',  ( -7.921791253741313987, -47.08507903579843656, -17.22412991407007254 ) ) ;
#391 = EDGE_CURVE ( 'NONE', #6478, #4633, #15029, .T. ) ;
#392 = CARTESIAN_POINT ( 'NONE',  ( -7.829332545557822876, -7.130382030772259405, 54.00231026484399166 ) ) ;
#393 = EDGE_CURVE ( 'NONE', #2126, #6515, #10210, .T. ) ;
#394 = EDGE_LOOP ( 'NONE', ( #13412, #6432, #8767, #12041 ) ) ;
#395 = CARTESIAN_POINT ( 'NONE',  ( -10.27295246487022240, -6.088325032597582620, 56.85231026484398598 ) ) ;
#396 = ORIENTED_EDGE ( 'NONE', *, *, #11686, .F. ) ;
#398 = EDGE_LOOP ( 'NONE', ( #9560, #11347, #6065, #9121, #218, #1341, #14177, #5755, #9138, #2250, #8409, #841, #3009, #12196, #3012, #215, #6805, #10450, #11048, #3124, #8673, #4543, #13338, #1727, #6461, #20, #10686, #9196, #12441, #10883, #7309, #5437, #1481, #5195, #2738, #14936, #13462, #1244, #15109, #5142, #4772, #10095, #7336, #13120, #462, #7253, #2154, #14889, #4656, #3287, #6719, #5542, #5255, #5721, #5056, #7185, #6602, #11840, #12110, #9524, #2176, #7888, #3618, #840, #2267, #1060, #11943, #5202, #12654, #8703, #7274, #1364, #12906, #13394, #10919, #9271, #428, #5605, #11, #4999, #1774, #7100, #4480, #2417, #10113, #7120, #11578, #6781, #13390, #6535, #3685, #6336, #9887, #10899, #2644, #11457 ) ) ;
#397 = CARTESIAN_POINT ( 'NONE',  ( -33.53898029810832782, -41.37673382704548430, -13.37373704449904999 ) ) ;
#399 = ORIENTED_EDGE ( 'NONE', *, *, #9618, .F. ) ;
#400 = PLANE ( 'NONE',  #4949 ) ;
#401 = CARTESIAN_POINT ( 'NONE',  ( -7.426192534185826588, -13.67980128487994129, 56.85231026484400019 ) ) ;
#402 = CYLINDRICAL_SURFACE ( 'NONE', #9146, 1.249999999999999778 ) ;
#403 = CIRCLE ( 'NONE', #7222, 9.974999999999999645 ) ;
#404 = CARTESIAN_POINT ( 'NONE',  ( -14.19604964772364220, -3.572340267249467960, 61.69496804699286940 ) ) ;
#405 = DIRECTION ( 'NONE',  ( 0.000000000000000000, 0.000000000000000000, -1.000000000000000000 ) ) ;
#406 = ADVANCED_FACE ( 'NONE', ( #6600 ), #11286, .T. ) ;
#407 = CARTESIAN_POINT ( 'NONE',  ( -8.639554752241616953, -9.247137322136806503, 57.00231026484399166 ) ) ;
#408 = CARTESIAN_POINT ( 'NONE',  ( -15.83606446161809522, -16.37446674635458166, 56.75231026484397745 ) ) ;
#409 = ORIENTED_EDGE ( 'NONE', *, *, #7322, .F. ) ;
#410 = SHAPE_REPRESENTATION ( 'Cross Slide Block', ( #6789 ), #14627 ) ;
#411 = DIRECTION ( 'NONE',  ( 0.000000000000000000, -1.000000000000000000, -1.224646799147350002E-16 ) ) ;
#412 = ORIENTED_EDGE ( 'NONE', *, *, #3457, .F. ) ;
#413 = VERTEX_POINT ( 'NONE', #3179 ) ;
#414 = CARTESIAN_POINT ( 'NONE',  ( -17.86883904694317593, -3.817807045405069655, 56.85231026484398598 ) ) ;
#415 = VERTEX_POINT ( 'NONE', #9058 ) ;
#416 = ORIENTED_EDGE ( 'NONE', *, *, #10394, .T. ) ;
#417 = CARTESIAN_POINT ( 'NONE',  ( -15.49969986081092088, -13.50737899243822504, 57.00231026484397745 ) ) ;
#418 = EDGE_CURVE ( 'NONE', #12386, #5342, #12547, .T. ) ;
#419 = DIRECTION ( 'NONE',  ( 0.000000000000000000, -1.000000000000000000, -1.224646799147350002E-16 ) ) ;
#420 = DIRECTION ( 'NONE',  ( -8.018662683283438208E-16, 5.975035461963189015E-16, 1.000000000000000000 ) ) ;
#421 = VECTOR ( 'NONE', #8848, 1000.000000000000000 ) ;
#422 = DIRECTION ( 'NONE',  ( 1.000000000000000275E-15, -0.9823027872370664326, 0.1872998510044542042 ) ) ;
#423 = PRODUCT_DEFINITION_SHAPE ( 'NONE', 'NONE',  #14249 ) ;
#425 = CARTESIAN_POINT ( 'NONE',  ( -36.12103303905597329, 5.873878172627213345, 19.00766998042008993 ) ) ;
#424 = CARTESIAN_POINT ( 'NONE',  ( -7.499751500627866996, -49.00722532478560822, -5.529656340655102476 ) ) ;
#426 = ORIENTED_EDGE ( 'NONE', *, *, #5229, .F. ) ;
#427 = CARTESIAN_POINT ( 'NONE',  ( 2.500300139188998738, -46.50737899243799944, 22.00231026484399877 ) ) ;
#428 = ORIENTED_EDGE ( 'NONE', *, *, #3740, .T. ) ;
#429 = CARTESIAN_POINT ( 'NONE',  ( -25.49948389380865166, -14.04222171988956980, 60.35420473814775733 ) ) ;
#430 = ORIENTED_EDGE ( 'NONE', *, *, #211, .T. ) ;
#431 = ORIENTED_EDGE ( 'NONE', *, *, #15117, .F. ) ;
#432 = PLANE ( 'NONE',  #8349 ) ;
#433 = ORIENTED_EDGE ( 'NONE', *, *, #11484, .F. ) ;
#434 = CIRCLE ( 'NONE', #12892, 6.000000000000001776 ) ;
#435 = ADVANCED_FACE ( 'NONE', ( #3259 ), #11815, .F. ) ;
#436 = CARTESIAN_POINT ( 'NONE',  ( -15.54961651457173488, -13.51026476396819831, 56.85231026484398598 ) ) ;
#437 = CARTESIAN_POINT ( 'NONE',  ( -9.503465417293824657, -21.51087798686868169, 56.51956357228300476 ) ) ;
#438 = AXIS2_PLACEMENT_3D ( 'NONE', #1903, #3121, #4272 ) ;
#439 = FACE_OUTER_BOUND ( 'NONE', #5049, .T. ) ;
#440 = CARTESIAN_POINT ( 'NONE',  ( -6.488891646287396675, -12.42729319905174634, 57.00231026484399166 ) ) ;
#441 = AXIS2_PLACEMENT_3D ( 'NONE', #10410, #13028, #12801 ) ;
#442 = ORIENTED_EDGE ( 'NONE', *, *, #8119, .T. ) ;
#443 = CARTESIAN_POINT ( 'NONE',  ( -18.18846581869435042, -17.11577719991577595, 48.00231026484398456 ) ) ;
#444 = DIRECTION ( 'NONE',  ( 0.000000000000000000, -2.168404344971007882E-16, 1.000000000000000000 ) ) ;
#445 = EDGE_LOOP ( 'NONE', ( #12637, #4168, #4808, #409 ) ) ;
#446 = LINE ( 'NONE', #6386, #12519 ) ;
#447 = SURFACE_SIDE_STYLE ('',( #4964 ) ) ;
#448 = ORIENTED_EDGE ( 'NONE', *, *, #2178, .F. ) ;
#449 = CARTESIAN_POINT ( 'NONE',  ( -14.10579935493720782, -22.47500361547664127, 56.85231026484400019 ) ) ;
#450 = ORIENTED_EDGE ( 'NONE', *, *, #10660, .T. ) ;
#451 = DIRECTION ( 'NONE',  ( -0.4491835085186243748, -0.8934395198752397294, 1.736481776669299976E-16 ) ) ;
#452 = AXIS2_PLACEMENT_3D ( 'NONE', #12447, #14978, #15050 ) ;
#453 = VECTOR ( 'NONE', #13350, 1000.000000000000000 ) ;
#454 = EDGE_CURVE ( 'NONE', #4959, #9649, #332, .T. ) ;
#455 = AXIS2_PLACEMENT_3D ( 'NONE', #5725, #6934, #3584 ) ;
#456 = AXIS2_PLACEMENT_3D ( 'NONE', #14616, #2988, #10880 ) ;
#457 = FACE_OUTER_BOUND ( 'NONE', #11590, .T. ) ;
#458 = ADVANCED_FACE ( 'NONE', ( #3557 ), #9287, .T. ) ;
#459 = CARTESIAN_POINT ( 'NONE',  ( -7.879287384819388507, -47.08648443922106708, 17.06717620651851064 ) ) ;
#460 = CARTESIAN_POINT ( 'NONE',  ( 18.30059761021155040, -28.74139264981273456, 7.969802569063922704 ) ) ;
#461 = DIRECTION ( 'NONE',  ( -1.000000000000000000, 1.291538348938060198E-32, -1.054621095516909827E-16 ) ) ;
#462 = ORIENTED_EDGE ( 'NONE', *, *, #5462, .T. ) ;
#463 = DIRECTION ( 'NONE',  ( 0.000000000000000000, 0.000000000000000000, 1.000000000000000000 ) ) ;
#464 = CARTESIAN_POINT ( 'NONE',  ( -6.766506000727597225, -11.03906478995046214, 57.00231026484399166 ) ) ;
#465 = ORIENTED_EDGE ( 'NONE', *, *, #14636, .T. ) ;
#466 = DIRECTION ( 'NONE',  ( 1.000000000000000000, 1.201369187114119994E-15, 9.616040805000176517E-16 ) ) ;
#467 = EDGE_LOOP ( 'NONE', ( #13198, #13690 ) ) ;
#469 = ORIENTED_EDGE ( 'NONE', *, *, #1383, .F. ) ;
#468 = CARTESIAN_POINT ( 'NONE',  ( -37.32932784798677517, -37.10979894228395182, -10.99641364132881094 ) ) ;
#470 = VERTEX_POINT ( 'NONE', #44 ) ;
#471 = DIRECTION ( 'NONE',  ( 0.02283895005205794151, -0.9997391571607663341, 6.156614753256579139E-16 ) ) ;
#472 = CYLINDRICAL_SURFACE ( 'NONE', #13911, 10.00000000000000000 ) ;
#473 = ADVANCED_FACE ( 'NONE', ( #4936 ), #4865, .T. ) ;
#474 = EDGE_CURVE ( 'NONE', #5883, #11022, #2563, .T. ) ;
#475 = CARTESIAN_POINT ( 'NONE',  ( -9.452813543643186378, -20.27468391147722926, 56.85231026484400019 ) ) ;
#476 = EDGE_CURVE ( 'NONE', #15009, #8801, #12188, .T. ) ;
#477 = CYLINDRICAL_SURFACE ( 'NONE', #7239, 2.500000000000002220 ) ;
#478 = APPLICATION_PROTOCOL_DEFINITION ( 'draft international standard', 'automotive_design', 1998, #13111 ) ;
#479 = CARTESIAN_POINT ( 'NONE',  ( -18.09969986081100046, -107.0941666664711676, -4.789471339975055919 ) ) ;
#480 = PLANE ( 'NONE',  #13859 ) ;
#481 = AXIS2_PLACEMENT_3D ( 'NONE', #6278, #6351, #14474 ) ;
#482 = EDGE_CURVE ( 'NONE', #8690, #13854, #8445, .T. ) ;
#483 = CARTESIAN_POINT ( 'NONE',  ( -7.506367692296740834, -44.17806943360024974, 45.42009090809814609 ) ) ;
#484 = CARTESIAN_POINT ( 'NONE',  ( 22.00030013918900096, -27.00737899243800300, 27.46206422150099868 ) ) ;
#485 = ORIENTED_EDGE ( 'NONE', *, *, #2144, .T. ) ;
#486 = CARTESIAN_POINT ( 'NONE',  ( -1.425463962227843995, -54.93314309385483796, 54.32987364559348009 ) ) ;
#487 = EDGE_LOOP ( 'NONE', ( #1278, #9865 ) ) ;
#488 = ORIENTED_EDGE ( 'NONE', *, *, #10656, .F. ) ;
#489 = PLANE ( 'NONE',  #5895 ) ;
#490 = ORIENTED_EDGE ( 'NONE', *, *, #13327, .T. ) ;
#491 = DIRECTION ( 'NONE',  ( -0.1908089953765440827, -0.9802818975087835840, 0.05137439731980028568 ) ) ;
#492 = EDGE_CURVE ( 'NONE', #11705, #3542, #8135, .T. ) ;
#493 = VECTOR ( 'NONE', #2962, 1000.000000000000000 ) ;
#494 = DIRECTION ( 'NONE',  ( -8.018662683283438208E-16, 5.975035461963189015E-16, 1.000000000000000000 ) ) ;
#495 = DIRECTION ( 'NONE',  ( 8.018662683283438208E-16, -5.975035461963189015E-16, -1.000000000000000000 ) ) ;
#496 =( BOUNDED_CURVE ( )  B_SPLINE_CURVE ( 3, ( #7778, #12464, #6703, #906 ),
 .UNSPECIFIED., .F., .F. ) 
 B_SPLINE_CURVE_WITH_KNOTS ( ( 4, 4 ),
 ( 1.570796326794895004, 3.141592653589793116 ),
 .UNSPECIFIED. ) 
 CURVE ( )  GEOMETRIC_REPRESENTATION_ITEM ( )  RATIONAL_B_SPLINE_CURVE ( ( 1.000000000000000000, 0.8047378541243646044, 0.8047378541243646044, 1.000000000000000000 ) ) 
 REPRESENTATION_ITEM ( '' )  );
#497 = FACE_OUTER_BOUND ( 'NONE', #9125, .T. ) ;
#498 = ORIENTED_EDGE ( 'NONE', *, *, #6384, .T. ) ;
#499 = DIRECTION ( 'NONE',  ( 0.000000000000000000, -1.000000000000000000, -1.224646799147350002E-16 ) ) ;
#500 = DIRECTION ( 'NONE',  ( -8.018662683283438208E-16, 5.975035461963189015E-16, 1.000000000000000000 ) ) ;
#501 = ORIENTED_EDGE ( 'NONE', *, *, #8338, .F. ) ;
#502 = ORIENTED_EDGE ( 'NONE', *, *, #12063, .T. ) ;
#503 = EDGE_CURVE ( 'NONE', #10963, #7558, #4786, .T. ) ;
#504 = CARTESIAN_POINT ( 'NONE',  ( -21.84916367058906772, -49.38105347906694931, 56.46124168193669135 ) ) ;
#505 = VERTEX_POINT ( 'NONE', #5991 ) ;
#506 = CARTESIAN_POINT ( 'NONE',  ( -25.21423696146293736, -11.24278324042066046, 54.00231026484397745 ) ) ;
#507 = DIRECTION ( 'NONE',  ( 1.000000000000000000, 1.201369187114119994E-15, 9.616040805000176517E-16 ) ) ;
#508 = DIRECTION ( 'NONE',  ( -1.000000000000000000, -1.201369187114119994E-15, -9.616040805000176517E-16 ) ) ;
#509 = CARTESIAN_POINT ( 'NONE',  ( 4.185908152460800835, 11.99262100756689620, 32.26206422150099939 ) ) ;
#510 = CARTESIAN_POINT ( 'NONE',  ( 13.85920135429429934, -23.75737899243800300, 43.21206422150100224 ) ) ;
#511 = ORIENTED_EDGE ( 'NONE', *, *, #9818, .F. ) ;
#512 = CARTESIAN_POINT ( 'NONE',  ( -11.08622897860377954, -4.561882931743225456, 56.85231026484398598 ) ) ;
#513 = CARTESIAN_POINT ( 'NONE',  ( -33.37394235882850069, 7.183219930803497633, 30.65500261342018007 ) ) ;
#514 = EDGE_LOOP ( 'NONE', ( #9562, #13979, #13683, #11446 ) ) ;
#515 = EDGE_CURVE ( 'NONE', #12112, #5496, #126, .T. ) ;
#516 = CARTESIAN_POINT ( 'NONE',  ( 21.99139210015182755, -23.86155550811809078, 25.05589765920358403 ) ) ;
#517 = DIRECTION ( 'NONE',  ( -8.018662683283438208E-16, 5.975035461963189015E-16, 1.000000000000000000 ) ) ;
#518 = ORIENTED_EDGE ( 'NONE', *, *, #13012, .T. ) ;
#519 = LINE ( 'NONE', #449, #1066 ) ;
#520 = ORIENTED_EDGE ( 'NONE', *, *, #7971, .F. ) ;
#521 = CARTESIAN_POINT ( 'NONE',  ( -7.838590061662593200, -46.81644859005926662, 21.98773677246508740 ) ) ;
#522 = VECTOR ( 'NONE', #10897, 1000.000000000000114 ) ;
#523 = FACE_OUTER_BOUND ( 'NONE', #3562, .T. ) ;
#524 = CARTESIAN_POINT ( 'NONE',  ( -7.426192534185826588, -13.67980128487993952, 57.00231026484399166 ) ) ;
#525 = DIRECTION ( 'NONE',  ( -5.000000000000000389E-16, 0.4999999999999998890, 0.8660254037844387076 ) ) ;
#526 = CARTESIAN_POINT ( 'NONE',  ( -14.61203582816999891, -107.9151965264422586, -6.615812085103268458 ) ) ;
#527 = ORIENTED_EDGE ( 'NONE', *, *, #9531, .T. ) ;
#528 = CARTESIAN_POINT ( 'NONE',  ( 6.045543233663400073, 12.99262100756199878, 32.26206422150099939 ) ) ;
#529 = LINE ( 'NONE', #4977, #7993 ) ;
#530 = AXIS2_PLACEMENT_3D ( 'NONE', #12947, #6943, #12 ) ;
#531 = EDGE_CURVE ( 'NONE', #12074, #14723, #3633, .T. ) ;
#532 = VERTEX_POINT ( 'NONE', #13131 ) ;
#533 = ORIENTED_EDGE ( 'NONE', *, *, #1466, .T. ) ;
#535 = EDGE_LOOP ( 'NONE', ( #3862, #9614, #2971, #6742 ) ) ;
#534 = DIRECTION ( 'NONE',  ( -1.000000000000000078E-15, 1.000000000000000000, 0.000000000000000000 ) ) ;
#536 = ORIENTED_EDGE ( 'NONE', *, *, #10912, .T. ) ;
#537 = DIRECTION ( 'NONE',  ( 0.1165201156931293391, 0.9931883319083343320, -4.999999999999998416E-16 ) ) ;
#538 = DIRECTION ( 'NONE',  ( -0.9673062255102924389, 0.2536112499260064768, -9.271838545667833343E-16 ) ) ;
#539 = VECTOR ( 'NONE', #6589, 999.9999999999998863 ) ;
#540 = CARTESIAN_POINT ( 'NONE',  ( -33.06833922757078881, 8.472784761962646627, 16.97712202220791156 ) ) ;
#541 = VECTOR ( 'NONE', #2213, 1000.000000000000000 ) ;
#542 = PRODUCT_DEFINITION_SHAPE ( 'NONE', 'NONE',  #10680 ) ;
#543 = CONICAL_SURFACE ( 'NONE', #12526, 23.00000000000000000, 1.047197551196598297 ) ;
#544 = CARTESIAN_POINT ( 'NONE',  ( -5.526612771747954511, -13.70272205979775215, 57.00231026484399166 ) ) ;
#545 = B_SPLINE_CURVE_WITH_KNOTS ( 'NONE', 3,
 ( #4916, #1388, #10721, #3763 ),
 .UNSPECIFIED., .F., .F.,
 ( 4, 4 ),
 ( 0.000000000000000000, 1.000000000000000000 ),
 .UNSPECIFIED. ) ;
#546 = CARTESIAN_POINT ( 'NONE',  ( -5.499699860811000818, -46.50737899243799944, 22.50231026484399877 ) ) ;
#547 = CARTESIAN_POINT ( 'NONE',  ( -15.64858178355719964, -107.2459911536667505, -7.686455132697844306 ) ) ;
#548 = FACE_OUTER_BOUND ( 'NONE', #4580, .T. ) ;
#549 = EDGE_CURVE ( 'NONE', #3237, #9332, #11203, .T. ) ;
#550 = CIRCLE ( 'NONE', #2008, 5.000000000000000000 ) ;
#551 = VERTEX_POINT ( 'NONE', #4711 ) ;
#552 = AXIS2_PLACEMENT_3D ( 'NONE', #3432, #12781, #11690 ) ;
#553 = ORIENTED_EDGE ( 'NONE', *, *, #12726, .F. ) ;
#554 = ORIENTED_EDGE ( 'NONE', *, *, #8317, .F. ) ;
#555 = ORIENTED_EDGE ( 'NONE', *, *, #2708, .T. ) ;
#556 = AXIS2_PLACEMENT_3D ( 'NONE', #9070, #5629, #975 ) ;
#557 = CIRCLE ( 'NONE', #1776, 9.974999999999999645 ) ;
#558 = EDGE_CURVE ( 'NONE', #9278, #700, #3139, .T. ) ;
#559 = DIRECTION ( 'NONE',  ( 0.000000000000000000, 1.508455196501571429E-16, -1.000000000000000000 ) ) ;
#560 = VERTEX_POINT ( 'NONE', #197 ) ;
#561 = DIRECTION ( 'NONE',  ( -0.9183863840214728791, -0.3956847857120156520, -4.999999999999998416E-16 ) ) ;
#562 = EDGE_CURVE ( 'NONE', #12498, #8595, #5230, .T. ) ;
#563 = PLANE ( 'NONE',  #11485 ) ;
#564 = CARTESIAN_POINT ( 'NONE',  ( -9.204203523554131294, -8.449911655164932256, 56.85231026484398598 ) ) ;
#565 = AXIS2_PLACEMENT_3D ( 'NONE', #1376, #13021, #11699 ) ;
#567 = CARTESIAN_POINT ( 'NONE',  ( -36.32388817133784897, 5.776599650201116098, 19.12436011050695939 ) ) ;
#566 = CARTESIAN_POINT ( 'NONE',  ( -31.79969986081099975, 3.992621007561997892, 24.21206422150099868 ) ) ;
#568 = EDGE_CURVE ( 'NONE', #9210, #8324, #1106, .T. ) ;
#569 = VERTEX_POINT ( 'NONE', #273 ) ;
#570 = CARTESIAN_POINT ( 'NONE',  ( -15.49969986081099371, -26.50737899243800300, 56.85231026484400019 ) ) ;
#571 = ADVANCED_FACE ( 'NONE', ( #9596, #6439 ), #9749, .F. ) ;
#572 = VERTEX_POINT ( 'NONE', #7518 ) ;
#573 = CARTESIAN_POINT ( 'NONE',  ( -5.499699860810998153, -46.50737899243799944, -2.497689735156003010 ) ) ;
#574 = ORIENTED_EDGE ( 'NONE', *, *, #9034, .T. ) ;
#575 = ORIENTED_EDGE ( 'NONE', *, *, #9073, .T. ) ;
#576 = CARTESIAN_POINT ( 'NONE',  ( -18.33272512729327985, -51.99348705970457729, 56.89592189784066534 ) ) ;
#577 = ORIENTED_EDGE ( 'NONE', *, *, #2278, .F. ) ;
#578 = CARTESIAN_POINT ( 'NONE',  ( -14.97634376076197427, -36.52016005446672864, 56.99957717010889269 ) ) ;
#579 = VECTOR ( 'NONE', #5511, 1000.000000000000000 ) ;
#580 = CIRCLE ( 'NONE', #12062, 9.974999999999999645 ) ;
#581 = AXIS2_PLACEMENT_3D ( 'NONE', #11592, #5841, #967 ) ;
#582 = CARTESIAN_POINT ( 'NONE',  ( 4.847130973315482372, 6.005480809351509741, 18.85628166566612407 ) ) ;
#583 = CARTESIAN_POINT ( 'NONE',  ( -20.87112600995946465, -106.1573670789699406, -5.659460905592496260 ) ) ;
#584 = CARTESIAN_POINT ( 'NONE',  ( -15.61203582817000068, -106.1207381828630929, -5.933688532728892184 ) ) ;
#585 = AXIS2_PLACEMENT_3D ( 'NONE', #3960, #12144, #9989 ) ;
#586 = DIRECTION ( 'NONE',  ( -8.018662683283438208E-16, 5.975035461963189015E-16, 1.000000000000000000 ) ) ;
#587 = CARTESIAN_POINT ( 'NONE',  ( -19.99969986081099904, -13.50737899243800122, 6.712064221500998684 ) ) ;
#588 = ORIENTED_EDGE ( 'NONE', *, *, #6627, .F. ) ;
#589 = DIRECTION ( 'NONE',  ( -3.839882694219489529E-17, 1.000000000000000000, 0.000000000000000000 ) ) ;
#590 = EDGE_CURVE ( 'NONE', #5768, #8983, #12195, .T. ) ;
#591 = CARTESIAN_POINT ( 'NONE',  ( -12.69917084408742269, -12.16466883763078144, 57.00231026484397745 ) ) ;
#592 = EDGE_LOOP ( 'NONE', ( #1009, #7727, #14645, #8081 ) ) ;
#593 = EDGE_CURVE ( 'NONE', #3314, #3333, #9963, .T. ) ;
#594 = CARTESIAN_POINT ( 'NONE',  ( 21.89436017916797894, -25.37669890083672541, 21.39281022185563330 ) ) ;
#595 = PLANE ( 'NONE',  #7643 ) ;
#596 = AXIS2_PLACEMENT_3D ( 'NONE', #4175, #9910, #7609 ) ;
#597 = ORIENTED_EDGE ( 'NONE', *, *, #4963, .F. ) ;
#598 = LINE ( 'NONE', #13310, #13985 ) ;
#599 = VECTOR ( 'NONE', #12678, 1000.000000000000114 ) ;
#600 = FACE_OUTER_BOUND ( 'NONE', #3661, .T. ) ;
#601 = EDGE_CURVE ( 'NONE', #7394, #8222, #3773, .T. ) ;
#602 = CARTESIAN_POINT ( 'NONE',  ( -24.36945568363038461, -11.58678490633884373, 56.85231026484398598 ) ) ;
#603 = CARTESIAN_POINT ( 'NONE',  ( 2.500300139188996962, -46.50737899243799944, 41.50231026484399166 ) ) ;
#604 = DIRECTION ( 'NONE',  ( -8.018662683283439195E-16, 5.975035461963190001E-16, 1.000000000000000000 ) ) ;
#605 = ORIENTED_EDGE ( 'NONE', *, *, #6254, .F. ) ;
#606 = DIRECTION ( 'NONE',  ( -1.011922027653136551E-15, 1.000000000000000000, 0.000000000000000000 ) ) ;
#607 = CARTESIAN_POINT ( 'NONE',  ( -16.09969986081092941, -93.78236537426951713, -11.11889594355865185 ) ) ;
#608 = VECTOR ( 'NONE', #7086, 1000.000000000000000 ) ;
#609 = VERTEX_POINT ( 'NONE', #5087 ) ;
#611 = ORIENTED_EDGE ( 'NONE', *, *, #9222, .F. ) ;
#610 = CARTESIAN_POINT ( 'NONE',  ( -35.12686845230359722, -38.31628777931871355, -12.45116519455210202 ) ) ;
#612 = VERTEX_POINT ( 'NONE', #6137 ) ;
#613 = ADVANCED_BREP_SHAPE_REPRESENTATION ( '', ( #7461, #6789 ), #4860 ) ;
#614 = FACE_OUTER_BOUND ( 'NONE', #3144, .T. ) ;
#615 = ORIENTED_EDGE ( 'NONE', *, *, #11602, .F. ) ;
#616 = CARTESIAN_POINT ( 'NONE',  ( -22.67472226038933059, -17.21206232108429290, 56.85231026484398598 ) ) ;
#617 = LINE ( 'NONE', #14613, #11114 ) ;
#618 = VECTOR ( 'NONE', #14146, 1000.000000000000000 ) ;
#619 = EDGE_CURVE ( 'NONE', #13349, #1021, #9822, .T. ) ;
#620 = CARTESIAN_POINT ( 'NONE',  ( -15.49969986081099904, 22.99262100756200056, 24.21206422150099868 ) ) ;
#621 = CARTESIAN_POINT ( 'NONE',  ( -8.971570239337625097, -21.04953708182106453, 54.00231026484400587 ) ) ;
#622 = DIRECTION ( 'NONE',  ( -1.000000000000000078E-15, 1.000000000000000000, 0.000000000000000000 ) ) ;
#623 = CARTESIAN_POINT ( 'NONE',  ( -7.500891366873055688, -44.35589769198639942, 43.22203397690024218 ) ) ;
#624 = ORIENTED_EDGE ( 'NONE', *, *, #10374, .F. ) ;
#625 = DIRECTION ( 'NONE',  ( 8.018662683283438208E-16, -5.975035461963189015E-16, -1.000000000000000000 ) ) ;
#626 = VERTEX_POINT ( 'NONE', #2711 ) ;
#627 = CARTESIAN_POINT ( 'NONE',  ( -1.508527451665001351, -45.27812899243799194, -5.497689735156000346 ) ) ;
#629 = ORIENTED_EDGE ( 'NONE', *, *, #8780, .T. ) ;
#628 = LINE ( 'NONE', #12406, #4473 ) ;
#630 = ORIENTED_EDGE ( 'NONE', *, *, #6574, .F. ) ;
#631 = DIRECTION ( 'NONE',  ( 0.7953815700667045130, 0.6061090314441981430, 2.756373558170028881E-16 ) ) ;
#633 = VERTEX_POINT ( 'NONE', #356 ) ;
#632 = DIRECTION ( 'NONE',  ( 0.000000000000000000, 0.000000000000000000, -1.000000000000000000 ) ) ;
#634 = CARTESIAN_POINT ( 'NONE',  ( -12.52412891130166628, -10.11885649493944150, -13.17027540314590794 ) ) ;
#635 = ADVANCED_FACE ( 'NONE', ( #7365 ), #7594, .F. ) ;
#636 = LINE ( 'NONE', #10968, #4651 ) ;
#637 = DIRECTION ( 'NONE',  ( 0.9885168150181788960, -0.1511109077013150503, 8.829475928589270966E-16 ) ) ;
#638 = EDGE_CURVE ( 'NONE', #2290, #7645, #5016, .T. ) ;
#639 = CIRCLE ( 'NONE', #9181, 5.000000000000000000 ) ;
#641 = CARTESIAN_POINT ( 'NONE',  ( -33.37394235882850069, 7.183219930803497633, 17.76912582958182085 ) ) ;
#640 = DIRECTION ( 'NONE',  ( 0.2196982563774038943, 0.9755678736739584744, -4.067366430757999696E-16 ) ) ;
#642 = VERTEX_POINT ( 'NONE', #14489 ) ;
#643 = LINE ( 'NONE', #8596, #7755 ) ;
#644 = FACE_OUTER_BOUND ( 'NONE', #1193, .T. ) ;
#645 = VERTEX_POINT ( 'NONE', #4079 ) ;
#646 = ORIENTED_EDGE ( 'NONE', *, *, #10912, .F. ) ;
#647 = FACE_OUTER_BOUND ( 'NONE', #4000, .T. ) ;
#648 = EDGE_LOOP ( 'NONE', ( #4869, #13209, #1415, #10166, #10438, #12905, #14791, #3642, #7670 ) ) ;
#649 = CARTESIAN_POINT ( 'NONE',  ( -13.41733751443047318, -36.76536173621014569, 56.94798727393903448 ) ) ;
#650 = EDGE_CURVE ( 'NONE', #1508, #1539, #12937, .T. ) ;
#651 = DIRECTION ( 'NONE',  ( 0.000000000000000000, 1.000000000000000000, 1.224646799147350002E-16 ) ) ;
#652 = CARTESIAN_POINT ( 'NONE',  ( -7.902754534677060683, -18.47202114588016642, 57.00231026484399166 ) ) ;
#653 = ADVANCED_FACE ( 'NONE', ( #8814 ), #3427, .T. ) ;
#654 = AXIS2_PLACEMENT_3D ( 'NONE', #10348, #4542, #5827 ) ;
#655 = CARTESIAN_POINT ( 'NONE',  ( -16.91203582817000139, -106.9280785958314368, -4.859811251109669605 ) ) ;
#656 = EDGE_CURVE ( 'NONE', #2388, #14032, #13686, .T. ) ;
#657 = DIRECTION ( 'NONE',  ( 0.9918751611018171710, 0.1272150336605075427, 7.193398003386516820E-16 ) ) ;
#658 = FACE_OUTER_BOUND ( 'NONE', #3242, .T. ) ;
#659 = ORIENTED_EDGE ( 'NONE', *, *, #13177, .F. ) ;
#660 = DIRECTION ( 'NONE',  ( -8.018662683283438208E-16, 5.975035461963189015E-16, 1.000000000000000000 ) ) ;
#661 = ORIENTED_EDGE ( 'NONE', *, *, #914, .T. ) ;
#662 = EDGE_CURVE ( 'NONE', #1582, #10428, #4356, .T. ) ;
#663 = CARTESIAN_POINT ( 'NONE',  ( 21.85920135429435618, -26.79521804582964251, 20.96206422150099868 ) ) ;
#664 = CARTESIAN_POINT ( 'NONE',  ( -25.21423696146293736, -11.24278324042065869, 57.00231026484397745 ) ) ;
#665 = ORIENTED_EDGE ( 'NONE', *, *, #13327, .F. ) ;
#666 = STYLED_ITEM ( 'NONE', ( #380 ), #2648 ) ;
#667 = CARTESIAN_POINT ( 'NONE',  ( -20.33437667196779586, -7.039214636791314206, 57.00231026484397745 ) ) ;
#668 = PLANE ( 'NONE',  #10986 ) ;
#669 = EDGE_CURVE ( 'NONE', #6892, #5883, #6927, .T. ) ;
#670 = AXIS2_PLACEMENT_3D ( 'NONE', #8463, #2659, #7310 ) ;
#671 = FACE_OUTER_BOUND ( 'NONE', #6924, .T. ) ;
#672 = VECTOR ( 'NONE', #3759, 1000.000000000000000 ) ;
#673 = CARTESIAN_POINT ( 'NONE',  ( -22.55857771067089246, -13.99059064457067336, 56.85231026484398598 ) ) ;
#674 = LINE ( 'NONE', #5559, #2557 ) ;
#675 = ORIENTED_EDGE ( 'NONE', *, *, #3273, .T. ) ;
#676 = CARTESIAN_POINT ( 'NONE',  ( 13.85920135429429934, -27.00737899243800300, 46.46206422150100224 ) ) ;
#677 = CARTESIAN_POINT ( 'NONE',  ( -7.557949836157023427, -45.46309933671603432, -3.215436967628607867 ) ) ;
#678 = ORIENTED_EDGE ( 'NONE', *, *, #6782, .T. ) ;
#679 = VECTOR ( 'NONE', #12925, 1000.000000000000000 ) ;
#680 = CONICAL_SURFACE ( 'NONE', #9472, 1.769239858347549932, 0.8464846872172493430 ) ;
#682 = EDGE_LOOP ( 'NONE', ( #8653, #5006 ) ) ;
#681 = FACE_OUTER_BOUND ( 'NONE', #12815, .T. ) ;
#683 = ORIENTED_EDGE ( 'NONE', *, *, #15059, .F. ) ;
#684 = EDGE_CURVE ( 'NONE', #5678, #1019, #2058, .T. ) ;
#685 = VECTOR ( 'NONE', #13993, 1000.000000000000000 ) ;
#686 = VECTOR ( 'NONE', #8907, 1000.000000000000000 ) ;
#687 = CARTESIAN_POINT ( 'NONE',  ( -11.90127153857800302, -52.50737899243802786, 27.50231026484402719 ) ) ;
#688 = LINE ( 'NONE', #14986, #1664 ) ;
#689 = FACE_OUTER_BOUND ( 'NONE', #11088, .T. ) ;
#690 = DIRECTION ( 'NONE',  ( -1.000000000000000000, -1.000000000000000078E-15, -1.000000000000000078E-15 ) ) ;
#691 = CARTESIAN_POINT ( 'NONE',  ( -15.49968909271368211, -3.507379016232285096, 61.71092834827113194 ) ) ;
#692 = AXIS2_PLACEMENT_3D ( 'NONE', #11251, #12556, #6566 ) ;
#693 = DIRECTION ( 'NONE',  ( 8.018662683283438208E-16, -5.975035461963189015E-16, -1.000000000000000000 ) ) ;
#694 = CARTESIAN_POINT ( 'NONE',  ( -15.82213178366242978, -16.25570808313599258, 51.00231026484399166 ) ) ;
#695 = VECTOR ( 'NONE', #3479, 1000.000000000000000 ) ;
#696 = CARTESIAN_POINT ( 'NONE',  ( -10.39628701978575975, -6.002951807498697612, 57.00231026484397745 ) ) ;
#697 = CARTESIAN_POINT ( 'NONE',  ( -7.499699860810999041, -44.50737899243799944, 43.00231026484400587 ) ) ;
#698 = ORIENTED_EDGE ( 'NONE', *, *, #7230, .T. ) ;
#699 = LINE ( 'NONE', #12712, #5166 ) ;
#700 = VERTEX_POINT ( 'NONE', #2286 ) ;
#701 = FACE_OUTER_BOUND ( 'NONE', #3699, .T. ) ;
#703 = ORIENTED_EDGE ( 'NONE', *, *, #6588, .T. ) ;
#702 = CARTESIAN_POINT ( 'NONE',  ( -7.661871090851159138, -46.13481490855701139, -7.997691309909533253 ) ) ;
#704 = ORIENTED_EDGE ( 'NONE', *, *, #9052, .F. ) ;
#705 = VECTOR ( 'NONE', #1786, 1000.000000000000000 ) ;
#706 = EDGE_CURVE ( 'NONE', #7812, #276, #2547, .T. ) ;
#707 = DIRECTION ( 'NONE',  ( -0.9999272109403024578, 0.01206535623792159839, -8.090169943749490479E-16 ) ) ;
#709 = ORIENTED_EDGE ( 'NONE', *, *, #4943, .T. ) ;
#708 = DIRECTION ( 'NONE',  ( 0.000000000000000000, 0.000000000000000000, 1.000000000000000000 ) ) ;
#710 = PLANE ( 'NONE',  #9268 ) ;
#711 = DIRECTION ( 'NONE',  ( 8.018662683283438208E-16, -5.975035461963189015E-16, -1.000000000000000000 ) ) ;
#712 = FACE_OUTER_BOUND ( 'NONE', #3959, .T. ) ;
#713 = AXIS2_PLACEMENT_3D ( 'NONE', #10885, #7580, #9736 ) ;
#714 = PRODUCT_DEFINITION_FORMATION_WITH_SPECIFIED_SOURCE ( 'ANY', '', #10297, .NOT_KNOWN. ) ;
#715 = CARTESIAN_POINT ( 'NONE',  ( -12.72810521832141362, -22.14910990341453001, 56.85231026484400019 ) ) ;
#716 = CARTESIAN_POINT ( 'NONE',  ( -34.99969986081099904, -19.50737899243800300, -12.52892449124999885 ) ) ;
#717 = CIRCLE ( 'NONE', #11214, 2.999999999999999112 ) ;
#718 = ORIENTED_EDGE ( 'NONE', *, *, #13711, .T. ) ;
#719 = CARTESIAN_POINT ( 'NONE',  ( -14.19354049678269192, -21.47604090745013750, 57.00231026484399166 ) ) ;
#720 = LINE ( 'NONE', #573, #13845 ) ;
#721 = ORIENTED_EDGE ( 'NONE', *, *, #9534, .T. ) ;
#722 = EDGE_LOOP ( 'NONE', ( #6651, #10903 ) ) ;
#723 = EDGE_CURVE ( 'NONE', #11355, #1607, #5563, .T. ) ;
#724 = CARTESIAN_POINT ( 'NONE',  ( -19.51359857101742534, -51.44753102027924285, 56.78947505621691505 ) ) ;
#725 = ORIENTED_EDGE ( 'NONE', *, *, #11167, .T. ) ;
#726 = AXIS2_PLACEMENT_3D ( 'NONE', #13566, #10336, #938 ) ;
#727 = VECTOR ( 'NONE', #4187, 1000.000000000000114 ) ;
#728 = DIRECTION ( 'NONE',  ( -1.000000000000000000, 1.291538348938060198E-32, -1.054621095516909827E-16 ) ) ;
#729 = EDGE_CURVE ( 'NONE', #10731, #4396, #14907, .T. ) ;
#730 = DIRECTION ( 'NONE',  ( 0.000000000000000000, 1.000000000000000000, 0.000000000000000000 ) ) ;
#731 = PLANE ( 'NONE',  #6812 ) ;
#732 = CARTESIAN_POINT ( 'NONE',  ( 5.426450521647101510, 12.65779542994580353, 16.16206422150100153 ) ) ;
#733 = CARTESIAN_POINT ( 'NONE',  ( -20.18599136182623965, -36.50737899243796392, 11.50231026484396146 ) ) ;
#734 = DIRECTION ( 'NONE',  ( 1.000000000000000000, -1.291538348938060198E-32, 1.054621095516909827E-16 ) ) ;
#735 = ORIENTED_EDGE ( 'NONE', *, *, #7834, .F. ) ;
#736 = DIRECTION ( 'NONE',  ( 0.000000000000000000, 0.1872998510044495413, 0.9823027872370673208 ) ) ;
#737 = PLANE ( 'NONE',  #10590 ) ;
#738 = ORIENTED_EDGE ( 'NONE', *, *, #13177, .T. ) ;
#739 = PLANE ( 'NONE',  #6134 ) ;
#740 = EDGE_CURVE ( 'NONE', #13270, #11202, #9081, .T. ) ;
#741 = STYLED_ITEM ( 'NONE', ( #11809 ), #7566 ) ;
#743 = EDGE_CURVE ( 'NONE', #11608, #1039, #13759, .T. ) ;
#742 = CARTESIAN_POINT ( 'NONE',  ( 21.97315826285361595, -24.08605709633378567, 25.65191965223944237 ) ) ;
#744 = LINE ( 'NONE', #11372, #7897 ) ;
#745 = VERTEX_POINT ( 'NONE', #8076 ) ;
#746 = CARTESIAN_POINT ( 'NONE',  ( -100.5053766806731090, -107.1622034095863825, -5.012689735156086179 ) ) ;
#747 = EDGE_CURVE ( 'NONE', #1568, #4448, #14520, .T. ) ;
#748 = DIRECTION ( 'NONE',  ( 0.05771543059946733500, -0.9983330752162417054, 6.427876096865391919E-16 ) ) ;
#749 = EDGE_CURVE ( 'NONE', #5139, #2245, #3034, .T. ) ;
#750 = CARTESIAN_POINT ( 'NONE',  ( -15.49969986081099904, -13.50737899243800122, 61.71206422150099513 ) ) ;
#751 = AXIS2_PLACEMENT_3D ( 'NONE', #13106, #11949, #1467 ) ;
#752 = B_SPLINE_CURVE_WITH_KNOTS ( 'NONE', 3,
 ( #2088, #3384, #15008, #9112, #3309, #13862, #14858, #6728 ),
 .UNSPECIFIED., .F., .F.,
 ( 4, 2, 2, 4 ),
 ( 0.003401025496237318393, 0.003933919667760182350, 0.004200366753521614545, 0.004466813839283045873 ),
 .UNSPECIFIED. ) ;
#753 = DIRECTION ( 'NONE',  ( 1.982541115402064518E-15, -0.1872998510044552312, -0.9823027872370662106 ) ) ;
#754 = CARTESIAN_POINT ( 'NONE',  ( -22.64031343690345111, -17.27870339600297811, 56.85231026484398598 ) ) ;
#755 = ORIENTED_EDGE ( 'NONE', *, *, #9574, .T. ) ;
#756 = DIRECTION ( 'NONE',  ( 1.000000000000000000, 1.000000000000000078E-15, 0.000000000000000000 ) ) ;
#757 = DIRECTION ( 'NONE',  ( 0.5975035461963189576, 0.8018662683283437342, 0.000000000000000000 ) ) ;
#758 = ADVANCED_FACE ( 'NONE', ( #14979 ), #10465, .T. ) ;
#759 = ADVANCED_FACE ( 'NONE', ( #4504 ), #3350, .F. ) ;
#760 = ORIENTED_EDGE ( 'NONE', *, *, #4717, .T. ) ;
#762 = ORIENTED_EDGE ( 'NONE', *, *, #283, .F. ) ;
#761 = CARTESIAN_POINT ( 'NONE',  ( -33.81822260959295789, -40.24903322724137666, -13.21898423093114161 ) ) ;
#763 = ORIENTED_EDGE ( 'NONE', *, *, #11807, .F. ) ;
#764 = DIRECTION ( 'NONE',  ( 0.5975035461963189576, 0.8018662683283437342, 0.000000000000000000 ) ) ;
#765 = CARTESIAN_POINT ( 'NONE',  ( -12.67205704361948193, -51.99558085209910985, 56.89633976960556083 ) ) ;
#766 = DIRECTION ( 'NONE',  ( 1.000000000000000000, 1.201369187114119994E-15, 9.616040805000176517E-16 ) ) ;
#767 = CARTESIAN_POINT ( 'NONE',  ( -15.49969986081099904, -37.00737899243799944, 19.50231026484400232 ) ) ;
#768 = CARTESIAN_POINT ( 'NONE',  ( -15.49969986081100082, -19.50737899243800300, 19.50231026484399877 ) ) ;
#769 = VECTOR ( 'NONE', #4307, 1000.000000000000000 ) ;
#770 = FACE_OUTER_BOUND ( 'NONE', #1435, .T. ) ;
#771 = DIRECTION ( 'NONE',  ( -8.673617379884027583E-16, 1.000000000000000000, 0.000000000000000000 ) ) ;
#772 = FACE_OUTER_BOUND ( 'NONE', #10937, .T. ) ;
#773 = ORIENTED_EDGE ( 'NONE', *, *, #13542, .F. ) ;
#774 = CARTESIAN_POINT ( 'NONE',  ( 17.02198936008371533, -30.24703833648301554, 42.88401681784144870 ) ) ;
#775 = VERTEX_POINT ( 'NONE', #3503 ) ;
#776 = EDGE_LOOP ( 'NONE', ( #8468, #14143, #4177, #7794 ) ) ;
#777 = VERTEX_POINT ( 'NONE', #12850 ) ;
#778 = VECTOR ( 'NONE', #1871, 1000.000000000000000 ) ;
#779 = ADVANCED_FACE ( 'NONE', ( #2362 ), #6997, .T. ) ;
#780 = CARTESIAN_POINT ( 'NONE',  ( -7.794854316102236780, -46.66267709929380914, 17.00231091965724062 ) ) ;
#782 = ORIENTED_EDGE ( 'NONE', *, *, #10510, .F. ) ;
#781 = CARTESIAN_POINT ( 'NONE',  ( 2.105912444148304807, 8.250019247675099976, 17.06248425561910409 ) ) ;
#783 = CIRCLE ( 'NONE', #9322, 9.974999999999999645 ) ;
#784 = CARTESIAN_POINT ( 'NONE',  ( -19.55678615628314532, -20.48959216528617233, 57.00231026484397745 ) ) ;
#785 = CARTESIAN_POINT ( 'NONE',  ( -12.72810521832141362, -22.14910990341453001, 56.85231026484400019 ) ) ;
#786 = LINE ( 'NONE', #6578, #10259 ) ;
#787 = EDGE_CURVE ( 'NONE', #6222, #34, #13589, .T. ) ;
#788 = EDGE_CURVE ( 'NONE', #4102, #4546, #10127, .T. ) ;
#789 = AXIS2_PLACEMENT_3D ( 'NONE', #6840, #972, #4339 ) ;
#790 = AXIS2_PLACEMENT_3D ( 'NONE', #1874, #14724, #12284 ) ;
#791 = DIRECTION ( 'NONE',  ( -0.9885168150181790070, 0.1511109077013141622, -8.829475928589267021E-16 ) ) ;
#792 = AXIS2_PLACEMENT_3D ( 'NONE', #7913, #13894, #1044 ) ;
#793 = PRODUCT_DEFINITION_SHAPE ( 'NONE', 'NONE',  #7495 ) ;
#794 = CIRCLE ( 'NONE', #4212, 5.250000000000000888 ) ;
#795 = CARTESIAN_POINT ( 'NONE',  ( -15.49969986081099727, -57.00737899243800655, 2.502310264843997878 ) ) ;
#796 = ORIENTED_EDGE ( 'NONE', *, *, #4234, .T. ) ;
#797 = PLANE ( 'NONE',  #14704 ) ;
#798 = ORIENTED_EDGE ( 'NONE', *, *, #9757, .T. ) ;
#799 = DIRECTION ( 'NONE',  ( -8.018662683283438208E-16, 5.975035461963189015E-16, 1.000000000000000000 ) ) ;
#800 = ORIENTED_EDGE ( 'NONE', *, *, #7591, .F. ) ;
#801 = EDGE_LOOP ( 'NONE', ( #1209, #6569, #11149, #361 ) ) ;
#802 = CARTESIAN_POINT ( 'NONE',  ( 2.551851194784686250, -41.28719780953740326, 52.37162401788530985 ) ) ;
#803 = ORIENTED_EDGE ( 'NONE', *, *, #14109, .T. ) ;
#804 = CARTESIAN_POINT ( 'NONE',  ( -20.06287389993751447, -22.40558212242008196, 56.72366690358678909 ) ) ;
#805 = CIRCLE ( 'NONE', #7388, 4.499999999999998224 ) ;
#806 = AXIS2_PLACEMENT_3D ( 'NONE', #12633, #6793, #12710 ) ;
#807 = LINE ( 'NONE', #13439, #14531 ) ;
#808 = DIRECTION ( 'NONE',  ( 0.8772189822852974883, -0.4800904676395346682, 9.902680687415700047E-16 ) ) ;
#809 = ADVANCED_FACE ( 'NONE', ( #11215 ), #3022, .F. ) ;
#810 = CARTESIAN_POINT ( 'NONE',  ( 6.045543233663400073, 12.99262100756199878, 16.16206422150100153 ) ) ;
#811 = FACE_OUTER_BOUND ( 'NONE', #5285, .T. ) ;
#813 = CARTESIAN_POINT ( 'NONE',  ( -35.18530787408519700, 11.99262100756819827, 32.26206422150099939 ) ) ;
#812 = DIRECTION ( 'NONE',  ( -0.1165201156931293391, -0.9931883319083343320, 4.999999999999998416E-16 ) ) ;
#814 = ORIENTED_EDGE ( 'NONE', *, *, #6711, .T. ) ;
#815 = DIRECTION ( 'NONE',  ( 1.000000000000000000, -1.291538348938060198E-32, 1.054621095516909827E-16 ) ) ;
#816 = LINE ( 'NONE', #4179, #222 ) ;
#817 = ORIENTED_EDGE ( 'NONE', *, *, #4925, .F. ) ;
#818 = VERTEX_POINT ( 'NONE', #7533 ) ;
#819 = AXIS2_PLACEMENT_3D ( 'NONE', #10441, #15107, #1187 ) ;
#820 = CARTESIAN_POINT ( 'NONE',  ( 2.374542637206501272, 7.183219930803497633, 30.65500261342018007 ) ) ;
#821 = VECTOR ( 'NONE', #9559, 1000.000000000000000 ) ;
#822 = AXIS2_PLACEMENT_3D ( 'NONE', #13222, #373, #9613 ) ;
#823 = CARTESIAN_POINT ( 'NONE',  ( -19.05470409992778258, -37.32136930023363419, -17.83198480484461967 ) ) ;
#824 = LINE ( 'NONE', #134, #11341 ) ;
#825 = ORIENTED_EDGE ( 'NONE', *, *, #1377, .T. ) ;
#826 = CARTESIAN_POINT ( 'NONE',  ( -14.00594099532011683, -11.50271332161736915, 51.00231026484399166 ) ) ;
#827 = CARTESIAN_POINT ( 'NONE',  ( -15.61203582816999891, -107.1622375242508696, -7.140479451889716778 ) ) ;
#828 = VECTOR ( 'NONE', #1734, 1000.000000000000000 ) ;
#829 = ADVANCED_FACE ( 'NONE', ( #5322 ), #8908, .F. ) ;
#830 = DIRECTION ( 'NONE',  ( -0.7276687409742212953, -0.6859287159822015090, -1.736481776669299729E-16 ) ) ;
#831 = CARTESIAN_POINT ( 'NONE',  ( -6.405625242116715690, -17.60596799715947114, 54.00231026484400587 ) ) ;
#832 = LINE ( 'NONE', #11155, #5240 ) ;
#833 = ADVANCED_FACE ( 'NONE', ( #14511 ), #1957, .F. ) ;
#834 = ORIENTED_EDGE ( 'NONE', *, *, #12625, .T. ) ;
#835 = CARTESIAN_POINT ( 'NONE',  ( 2.500300139188999626, -46.50737899243799944, 42.00231026484399166 ) ) ;
#836 = FACE_OUTER_BOUND ( 'NONE', #6119, .T. ) ;
#837 = VECTOR ( 'NONE', #3403, 1000.000000000000000 ) ;
#838 = EDGE_LOOP ( 'NONE', ( #10150, #10101, #7348, #913, #13152 ) ) ;
#840 = ORIENTED_EDGE ( 'NONE', *, *, #4770, .F. ) ;
#839 = CARTESIAN_POINT ( 'NONE',  ( -15.16333526000375187, -10.64029123852186132, 56.75231026484397745 ) ) ;
#841 = ORIENTED_EDGE ( 'NONE', *, *, #7865, .F. ) ;
#842 = STYLED_ITEM ( 'NONE', ( #11744 ), #12764 ) ;
#843 = FACE_OUTER_BOUND ( 'NONE', #937, .T. ) ;
#844 = CARTESIAN_POINT ( 'NONE',  ( -15.49969986081100082, -110.0623785963297365, -0.7605796072322540402 ) ) ;
#845 = FACE_OUTER_BOUND ( 'NONE', #6168, .T. ) ;
#846 = DIRECTION ( 'NONE',  ( 0.000000000000000000, -1.000000000000000000, -1.224646799147350002E-16 ) ) ;
#847 = EDGE_CURVE ( 'NONE', #10705, #1908, #4099, .T. ) ;
#848 = CARTESIAN_POINT ( 'NONE',  ( -11.71495923925436955, -5.812446346369147143, 56.85231026484398598 ) ) ;
#849 = EDGE_CURVE ( 'NONE', #6240, #10757, #14803, .T. ) ;
#850 = VECTOR ( 'NONE', #9016, 1000.000000000000000 ) ;
#851 = CARTESIAN_POINT ( 'NONE',  ( -5.499699860811000818, -46.50737899243799944, 17.00231026484399877 ) ) ;
#852 = CARTESIAN_POINT ( 'NONE',  ( -8.561607448813433052, -9.375294326971793879, 56.85231026484400019 ) ) ;
#853 = CARTESIAN_POINT ( 'NONE',  ( -23.49646891012291050, -9.216349422280851300, 57.00231026484397745 ) ) ;
#854 = CARTESIAN_POINT ( 'NONE',  ( -17.47506273705024071, -21.33739760717825718, 56.85231026484400019 ) ) ;
#855 = VERTEX_POINT ( 'NONE', #11283 ) ;
#857 = ORIENTED_EDGE ( 'NONE', *, *, #5983, .F. ) ;
#856 = CARTESIAN_POINT ( 'NONE',  ( -5.859109405273538407, -10.94619944609606677, 56.85231026484400019 ) ) ;
#858 = VERTEX_POINT ( 'NONE', #4329 ) ;
#859 = CARTESIAN_POINT ( 'NONE',  ( 6.045543233663400073, 0.9926210075619987805, 16.16206422150100153 ) ) ;
#860 = ORIENTED_EDGE ( 'NONE', *, *, #8404, .T. ) ;
#861 = DIRECTION ( 'NONE',  ( -1.000000000000000000, 1.291538348938060198E-32, -1.054621095516909827E-16 ) ) ;
#862 = VECTOR ( 'NONE', #4969, 1000.000000000000114 ) ;
#863 = DIRECTION ( 'NONE',  ( 0.000000000000000000, 0.000000000000000000, 1.000000000000000000 ) ) ;
#864 = LINE ( 'NONE', #5521, #4901 ) ;
#865 = SHAPE_REPRESENTATION_RELATIONSHIP ( 'NONE' , 'NONE' ,  #10170, #613 ) ;
#866 = EDGE_CURVE ( 'NONE', #8946, #5900, #1818, .T. ) ;
#867 = ORIENTED_EDGE ( 'NONE', *, *, #6524, .T. ) ;
#868 = LINE ( 'NONE', #11344, #14453 ) ;
#869 = DIRECTION ( 'NONE',  ( 8.018662683283438208E-16, -5.975035461963189015E-16, -1.000000000000000000 ) ) ;
#870 = ORIENTED_EDGE ( 'NONE', *, *, #5351, .F. ) ;
#871 = CARTESIAN_POINT ( 'NONE',  ( -23.49969986081100259, -44.50737899243799944, 56.13904046828872652 ) ) ;
#872 = ORIENTED_EDGE ( 'NONE', *, *, #6198, .F. ) ;
#873 = CARTESIAN_POINT ( 'NONE',  ( -10.16926643994361967, -19.57302854922115287, 56.85231026484400019 ) ) ;
#874 = ORIENTED_EDGE ( 'NONE', *, *, #9818, .T. ) ;
#875 = ORIENTED_EDGE ( 'NONE', *, *, #14446, .F. ) ;
#876 = DIRECTION ( 'NONE',  ( 0.000000000000000000, -1.000000000000000000, -1.224646799147350002E-16 ) ) ;
#877 = DIRECTION ( 'NONE',  ( -0.9805849309054472940, -0.1960948578651647567, -6.691306063588586415E-16 ) ) ;
#878 = EDGE_LOOP ( 'NONE', ( #6994, #13171 ) ) ;
#880 = ADVANCED_FACE ( 'NONE', ( #811 ), #352, .T. ) ;
#879 = DIRECTION ( 'NONE',  ( -8.673617379884027583E-16, 1.000000000000000000, 0.000000000000000000 ) ) ;
#881 = CYLINDRICAL_SURFACE ( 'NONE', #14903, 8.000000000000000000 ) ;
#882 = CARTESIAN_POINT ( 'NONE',  ( 2.436724872642413331, 11.05255549920696012, 16.20867245923580313 ) ) ;
#883 = VECTOR ( 'NONE', #3949, 1000.000000000000000 ) ;
#884 = CARTESIAN_POINT ( 'NONE',  ( 15.61764008820435023, -24.36042187135127080, 3.281355806888882398 ) ) ;
#885 = CARTESIAN_POINT ( 'NONE',  ( -7.754930580632606762, -46.50765881518451295, 22.00225574842814424 ) ) ;
#887 = CARTESIAN_POINT ( 'NONE',  ( 3.683561516709968675, 6.562241739470401569, 30.13885157671532156 ) ) ;
#886 = CYLINDRICAL_SURFACE ( 'NONE', #3992, 2.500000000000002220 ) ;
#888 = ORIENTED_EDGE ( 'NONE', *, *, #9875, .T. ) ;
#889 = CARTESIAN_POINT ( 'NONE',  ( -21.24026693782044717, -7.828337292084670551, 56.85231026484398598 ) ) ;
#890 = DIRECTION ( 'NONE',  ( -1.000000000000000000, -1.000000000000000078E-15, 0.000000000000000000 ) ) ;
#891 = ORIENTED_EDGE ( 'NONE', *, *, #9996, .T. ) ;
#892 = ORIENTED_EDGE ( 'NONE', *, *, #11461, .F. ) ;
#893 = CARTESIAN_POINT ( 'NONE',  ( -11.58094331127308507, -5.879823872646938732, 56.85231026484398598 ) ) ;
#894 = LINE ( 'NONE', #10136, #2389 ) ;
#895 = AXIS2_PLACEMENT_3D ( 'NONE', #13622, #13924, #1219 ) ;
#896 = CARTESIAN_POINT ( 'NONE',  ( -15.53979317422733786, -13.47750381512840967, 56.85231026484398598 ) ) ;
#897 = ORIENTED_EDGE ( 'NONE', *, *, #7816, .T. ) ;
#898 = LINE ( 'NONE', #7919, #2506 ) ;
#899 = ADVANCED_FACE ( 'NONE', ( #8979, #11140 ), #4029, .T. ) ;
#900 = DIRECTION ( 'NONE',  ( -1.000000000000000000, 1.291538348938060198E-32, -1.054621095516909827E-16 ) ) ;
#901 = DIRECTION ( 'NONE',  ( -1.000000000000000000, 0.000000000000000000, 0.000000000000000000 ) ) ;
#902 = VECTOR ( 'NONE', #9320, 999.9999999999998863 ) ;
#903 = CARTESIAN_POINT ( 'NONE',  ( -15.49969986081092088, -13.50737899243822504, 57.00231026484397745 ) ) ;
#904 = CARTESIAN_POINT ( 'NONE',  ( -17.40065610530428586, -5.145404622917534532, 57.00231026484397745 ) ) ;
#905 = ORIENTED_EDGE ( 'NONE', *, *, #10838, .F. ) ;
#906 = CARTESIAN_POINT ( 'NONE',  ( -15.49969986081099904, -52.50737899243800655, -13.49768973515600656 ) ) ;
#907 = CARTESIAN_POINT ( 'NONE',  ( -18.09969986081099336, -109.5303206426348765, -10.29048042260499862 ) ) ;
#908 = VECTOR ( 'NONE', #6585, 1000.000000000000000 ) ;
#909 = VECTOR ( 'NONE', #11459, 1000.000000000000000 ) ;
#910 = ORIENTED_EDGE ( 'NONE', *, *, #13189, .T. ) ;
#912 = ORIENTED_EDGE ( 'NONE', *, *, #1524, .T. ) ;
#911 = CARTESIAN_POINT ( 'NONE',  ( -7.502222146387037327, -44.75835849886513529, 46.29929020896280178 ) ) ;
#913 = ORIENTED_EDGE ( 'NONE', *, *, #997, .F. ) ;
#914 = EDGE_CURVE ( 'NONE', #1019, #12480, #14071, .T. ) ;
#915 = DIRECTION ( 'NONE',  ( 8.018662683283438208E-16, -5.975035461963189015E-16, -1.000000000000000000 ) ) ;
#916 = CARTESIAN_POINT ( 'NONE',  ( -15.34686821047329808, -23.48120812104550481, 57.00231026484399166 ) ) ;
#917 = VECTOR ( 'NONE', #12215, 1000.000000000000000 ) ;
#918 = EDGE_CURVE ( 'NONE', #15017, #6821, #3177, .T. ) ;
#919 = DIRECTION ( 'NONE',  ( 0.000000000000000000, 1.000000000000000000, 1.224646799147350002E-16 ) ) ;
#920 = CARTESIAN_POINT ( 'NONE',  ( -7.949560932996365459, -47.15762953262321844, 42.08283266251152810 ) ) ;
#921 = CARTESIAN_POINT ( 'NONE',  ( -7.785174720008381399, -8.727488632615573394, 56.85231026484400019 ) ) ;
#922 = LINE ( 'NONE', #7863, #14085 ) ;
#923 = VECTOR ( 'NONE', #1746, 1000.000000000000000 ) ;
#924 = AXIS2_PLACEMENT_3D ( 'NONE', #9119, #4238, #5750 ) ;
#925 = DIRECTION ( 'NONE',  ( 0.000000000000000000, 0.000000000000000000, 1.000000000000000000 ) ) ;
#926 = DIRECTION ( 'NONE',  ( 0.8772189822852964891, -0.4800904676395362780, 9.902680687415700047E-16 ) ) ;
#927 = VECTOR ( 'NONE', #246, 1000.000000000000114 ) ;
#928 = ORIENTED_EDGE ( 'NONE', *, *, #12469, .F. ) ;
#929 = CARTESIAN_POINT ( 'NONE',  ( 15.30759700337437046, -29.22784282607966588, 45.59414329854286763 ) ) ;
#930 = ORIENTED_EDGE ( 'NONE', *, *, #418, .T. ) ;
#932 = ORIENTED_EDGE ( 'NONE', *, *, #12744, .T. ) ;
#931 = DIRECTION ( 'NONE',  ( 8.018662683283438208E-16, -5.975035461963189015E-16, -1.000000000000000000 ) ) ;
#933 = ORIENTED_EDGE ( 'NONE', *, *, #6988, .F. ) ;
#934 = EDGE_CURVE ( 'NONE', #6732, #13413, #5465, .T. ) ;
#935 = DIRECTION ( 'NONE',  ( 0.000000000000000000, 1.224646799147350002E-16, -1.000000000000000000 ) ) ;
#936 = EDGE_CURVE ( 'NONE', #12614, #1243, #12290, .T. ) ;
#937 = EDGE_LOOP ( 'NONE', ( #1043, #14759, #7080, #4736 ) ) ;
#938 = DIRECTION ( 'NONE',  ( 0.000000000000000000, 0.000000000000000000, -1.000000000000000000 ) ) ;
#939 = ADVANCED_FACE ( 'NONE', ( #1653 ), #8885, .T. ) ;
#940 = AXIS2_PLACEMENT_3D ( 'NONE', #10481, #5955, #3518 ) ;
#941 = LINE ( 'NONE', #3154, #7567 ) ;
#942 = EDGE_CURVE ( 'NONE', #1308, #14720, #2548, .T. ) ;
#943 = ORIENTED_EDGE ( 'NONE', *, *, #194, .F. ) ;
#944 = CARTESIAN_POINT ( 'NONE',  ( -7.813858722443190352, -47.64803766822263498, -7.722934107415373006 ) ) ;
#945 = CIRCLE ( 'NONE', #13899, 8.000000000000000000 ) ;
#946 = CYLINDRICAL_SURFACE ( 'NONE', #13032, 8.000000000000000000 ) ;
#947 = VERTEX_POINT ( 'NONE', #2336 ) ;
#948 = CARTESIAN_POINT ( 'NONE',  ( 17.85343114739217540, -24.33247860872462809, 41.35438736840348639 ) ) ;
#949 = ORIENTED_EDGE ( 'NONE', *, *, #5249, .F. ) ;
#950 = PLANE ( 'NONE',  #12385 ) ;
#951 = VERTEX_POINT ( 'NONE', #12745 ) ;
#952 = EDGE_LOOP ( 'NONE', ( #1627, #1662, #4143, #1716 ) ) ;
#953 = AXIS2_PLACEMENT_3D ( 'NONE', #1340, #3709, #1183 ) ;
#954 = CARTESIAN_POINT ( 'NONE',  ( 2.704135510968567857, -40.58388572175281439, 52.28758934844383077 ) ) ;
#955 = ADVANCED_FACE ( 'NONE', ( #11434 ), #13956, .F. ) ;
#956 = ORIENTED_EDGE ( 'NONE', *, *, #1466, .F. ) ;
#957 = B_SPLINE_CURVE_WITH_KNOTS ( 'NONE', 3,
 ( #7231, #11916, #1439, #3884, #6166, #3805 ),
 .UNSPECIFIED., .F., .F.,
 ( 4, 2, 4 ),
 ( 0.000000000000000000, 0.1440237844040733739, 0.2880475688081467478 ),
 .UNSPECIFIED. ) ;
#958 =( LENGTH_UNIT ( ) NAMED_UNIT ( * ) SI_UNIT ( .MILLI., .METRE. ) );
#959 = CARTESIAN_POINT ( 'NONE',  ( -10.59914214906130780, -90.60588013820681397, -7.696961324692049189 ) ) ;
#960 = EDGE_CURVE ( 'NONE', #7202, #3278, #2137, .T. ) ;
#961 = CARTESIAN_POINT ( 'NONE',  ( -7.557932192427426088, -45.46324534594638322, 21.78464076912158376 ) ) ;
#963 = CARTESIAN_POINT ( 'NONE',  ( 9.000300139189000959, -27.00737899243800300, 26.71206422150099868 ) ) ;
#962 = CARTESIAN_POINT ( 'NONE',  ( -15.49969986081099904, 1010.738102757665843, 24.21206422150112303 ) ) ;
#964 = VERTEX_POINT ( 'NONE', #3327 ) ;
#965 = PLANE ( 'NONE',  #1419 ) ;
#966 = AXIS2_PLACEMENT_3D ( 'NONE', #3927, #561, #13271 ) ;
#967 = DIRECTION ( 'NONE',  ( 0.000000000000000000, -1.508455196501571676E-16, 1.000000000000000000 ) ) ;
#968 = EDGE_LOOP ( 'NONE', ( #5953, #3847, #10193, #5384 ) ) ;
#969 = VECTOR ( 'NONE', #11746, 1000.000000000000114 ) ;
#970 = VERTEX_POINT ( 'NONE', #7821 ) ;
#971 = CARTESIAN_POINT ( 'NONE',  ( -18.64620844969664759, -109.4443699603185678, -0.1262635860074659000 ) ) ;
#972 = DIRECTION ( 'NONE',  ( -8.018662683283438208E-16, 5.975035461963189015E-16, 1.000000000000000000 ) ) ;
#973 = DIRECTION ( 'NONE',  ( 0.000000000000000000, 0.000000000000000000, 1.000000000000000000 ) ) ;
#974 = ORIENTED_EDGE ( 'NONE', *, *, #1401, .T. ) ;
#975 = DIRECTION ( 'NONE',  ( 0.000000000000000000, 0.1872998510044759646, 0.9823027872370621028 ) ) ;
#976 = LINE ( 'NONE', #4567, #14165 ) ;
#977 = VECTOR ( 'NONE', #12742, 1000.000000000000000 ) ;
#978 = CARTESIAN_POINT ( 'NONE',  ( -7.611722567307242393, -48.62974432432149285, 20.82618560148544518 ) ) ;
#979 = EDGE_CURVE ( 'NONE', #13413, #2196, #9368, .T. ) ;
#980 = EDGE_CURVE ( 'NONE', #8879, #2383, #6903, .T. ) ;
#981 = CARTESIAN_POINT ( 'NONE',  ( 7.000300139189000070, -19.50737899243800300, 24.21206422150099868 ) ) ;
#983 = ORIENTED_EDGE ( 'NONE', *, *, #9725, .T. ) ;
#982 = AXIS2_PLACEMENT_3D ( 'NONE', #10415, #14932, #7803 ) ;
#984 = CARTESIAN_POINT ( 'NONE',  ( -10.29813411369431719, -90.56073884152880282, -4.157226901606094316 ) ) ;
#985 =( BOUNDED_CURVE ( )  B_SPLINE_CURVE ( 3, ( #10218, #8919, #14893, #13522 ),
 .UNSPECIFIED., .F., .T. ) 
 B_SPLINE_CURVE_WITH_KNOTS ( ( 4, 4 ),
 ( 3.141592653589792672, 4.712388980384689674 ),
 .UNSPECIFIED. ) 
 CURVE ( )  GEOMETRIC_REPRESENTATION_ITEM ( )  RATIONAL_B_SPLINE_CURVE ( ( 1.000000000000000000, 0.8047378541243649375, 0.8047378541243649375, 1.000000000000000000 ) ) 
 REPRESENTATION_ITEM ( '' )  );
#986 = CARTESIAN_POINT ( 'NONE',  ( -37.63784331376448478, 5.145091203786375189, 28.44116034148276739 ) ) ;
#987 = DIRECTION ( 'NONE',  ( -8.018662683283438208E-16, 5.975035461963189015E-16, 1.000000000000000000 ) ) ;
#988 = PLANE ( 'NONE',  #14150 ) ;
#989 = ORIENTED_EDGE ( 'NONE', *, *, #11826, .F. ) ;
#990 = EDGE_LOOP ( 'NONE', ( #3817, #11633, #11103, #5759 ) ) ;
#991 = DIRECTION ( 'NONE',  ( 0.1165201156931293391, 0.9931883319083343320, -4.999999999999998416E-16 ) ) ;
#992 = CARTESIAN_POINT ( 'NONE',  ( -8.703303756061691487, -48.73563719200068078, 56.38158717348355253 ) ) ;
#993 = AXIS2_PLACEMENT_3D ( 'NONE', #8792, #10014, #8719 ) ;
#994 = FACE_OUTER_BOUND ( 'NONE', #2243, .T. ) ;
#995 = CARTESIAN_POINT ( 'NONE',  ( -24.53816276005083452, -12.69040994830970703, 57.00231026484397745 ) ) ;
#996 = DIRECTION ( 'NONE',  ( 0.000000000000000000, 0.1872998510044759646, 0.9823027872370621028 ) ) ;
#997 = EDGE_CURVE ( 'NONE', #947, #12931, #5539, .T. ) ;
#998 = CYLINDRICAL_SURFACE ( 'NONE', #3816, 8.000000000000000000 ) ;
#999 = DIRECTION ( 'NONE',  ( 8.018662683283438208E-16, -5.975035461963189015E-16, -1.000000000000000000 ) ) ;
#1000 = CARTESIAN_POINT ( 'NONE',  ( -5.499699860811003482, -46.50737899243799944, 47.50231026484399877 ) ) ;
#1001 = ORIENTED_EDGE ( 'NONE', *, *, #9257, .F. ) ;
#1002 = CARTESIAN_POINT ( 'NONE',  ( 18.17361288855373758, -29.10044277972165716, 40.71597190168268554 ) ) ;
#1003 = VERTEX_POINT ( 'NONE', #11587 ) ;
#1004 = CARTESIAN_POINT ( 'NONE',  ( -22.70654572567255869, -20.40389968624657513, 57.00231026484397745 ) ) ;
#1006 = ORIENTED_EDGE ( 'NONE', *, *, #10301, .T. ) ;
#1005 = LINE ( 'NONE', #6798, #579 ) ;
#1007 = ORIENTED_EDGE ( 'NONE', *, *, #2915, .T. ) ;
#1008 = DIRECTION ( 'NONE',  ( -1.169602638241521591E-15, 0.1872998510044552312, 0.9823027872370662106 ) ) ;
#1009 = ORIENTED_EDGE ( 'NONE', *, *, #2438, .T. ) ;
#1010 = CARTESIAN_POINT ( 'NONE',  ( -23.43263029221230198, -15.01730109988151440, 57.00231026484397745 ) ) ;
#1011 = AXIS2_PLACEMENT_3D ( 'NONE', #9587, #2275, #13121 ) ;
#1012 = DIRECTION ( 'NONE',  ( 1.000000000000000000, 1.000000000000000078E-15, 0.000000000000000000 ) ) ;
#1013 = EDGE_CURVE ( 'NONE', #12480, #7811, #6818, .T. ) ;
#1014 = ORIENTED_EDGE ( 'NONE', *, *, #11151, .F. ) ;
#1015 = CARTESIAN_POINT ( 'NONE',  ( -23.49969986081100259, -44.50737899243799944, -17.13441993860073254 ) ) ;
#1016 = ADVANCED_FACE ( 'NONE', ( #14955 ), #11362, .F. ) ;
#1017 = ORIENTED_EDGE ( 'NONE', *, *, #13083, .T. ) ;
#1018 = CARTESIAN_POINT ( 'NONE',  ( -11.30335942247960546, -22.55676305576680818, 56.85231026484400019 ) ) ;
#1019 = VERTEX_POINT ( 'NONE', #12667 ) ;
#1020 = LINE ( 'NONE', #3317, #4324 ) ;
#1021 = VERTEX_POINT ( 'NONE', #6832 ) ;
#1022 = VERTEX_POINT ( 'NONE', #5762 ) ;
#1023 = PLANE ( 'NONE',  #4211 ) ;
#1024 = AXIS2_PLACEMENT_3D ( 'NONE', #8503, #14327, #12179 ) ;
#1025 = DIRECTION ( 'NONE',  ( 0.000000000000000000, 1.000000000000000000, 1.224646799147350002E-16 ) ) ;
#1026 = ORIENTED_EDGE ( 'NONE', *, *, #9723, .F. ) ;
#1027 = ADVANCED_FACE ( 'NONE', ( #4405 ), #7904, .F. ) ;
#1028 = CARTESIAN_POINT ( 'NONE',  ( -23.49969986081099904, -19.50737899243800300, 56.13904046828879757 ) ) ;
#1029 = DIRECTION ( 'NONE',  ( 8.018662683283438208E-16, -5.975035461963189015E-16, -1.000000000000000000 ) ) ;
#1030 = VECTOR ( 'NONE', #2943, 1000.000000000000000 ) ;
#1031 = LINE ( 'NONE', #3474, #9523 ) ;
#1032 = VECTOR ( 'NONE', #384, 1000.000000000000000 ) ;
#1033 = AXIS2_PLACEMENT_3D ( 'NONE', #10244, #1067, #9318 ) ;
#1034 = ADVANCED_FACE ( 'NONE', ( #4550 ), #10434, .T. ) ;
#1035 = ADVANCED_FACE ( 'NONE', ( #13129 ), #9671, .T. ) ;
#1036 = CARTESIAN_POINT ( 'NONE',  ( -23.49969986081100615, -39.82108749142274462, 24.18860176585925359 ) ) ;
#1038 = LINE ( 'NONE', #13736, #15097 ) ;
#1037 = PLANE ( 'NONE',  #13732 ) ;
#1039 = VERTEX_POINT ( 'NONE', #9593 ) ;
#1040 = CARTESIAN_POINT ( 'NONE',  ( -15.49969986081099904, 10.68321993080349941, 5.212064221501000461 ) ) ;
#1041 = DIRECTION ( 'NONE',  ( -8.018662683283439195E-16, 5.975035461963190001E-16, 1.000000000000000000 ) ) ;
#1042 = ORIENTED_EDGE ( 'NONE', *, *, #4702, .F. ) ;
#1043 = ORIENTED_EDGE ( 'NONE', *, *, #1994, .T. ) ;
#1044 = DIRECTION ( 'NONE',  ( 8.018662683283438208E-16, -5.975035461963189015E-16, -1.000000000000000000 ) ) ;
#1045 = CARTESIAN_POINT ( 'NONE',  ( -33.49969986081099904, -37.00737899243799944, 52.39987856403599409 ) ) ;
#1046 = AXIS2_PLACEMENT_3D ( 'NONE', #5420, #4205, #7634 ) ;
#1047 = ORIENTED_EDGE ( 'NONE', *, *, #2055, .T. ) ;
#1048 = CARTESIAN_POINT ( 'NONE',  ( -5.524802968312260809, -13.55273297815670119, 57.00231026484399166 ) ) ;
#1049 = VECTOR ( 'NONE', #12327, 999.9999999999998863 ) ;
#1050 = DIRECTION ( 'NONE',  ( 0.000000000000000000, 0.000000000000000000, -1.000000000000000000 ) ) ;
#1051 = ITEM_DEFINED_TRANSFORMATION ( 'NONE', 'NONE', #11709,  #6789 ) ;
#1052 = ADVANCED_FACE ( 'NONE', ( #6135 ), #8210, .T. ) ;
#1053 = CIRCLE ( 'NONE', #8629, 37.50000000000000000 ) ;
#1054 = DIRECTION ( 'NONE',  ( -1.050965490997517593E-15, 0.05233595624294359872, 0.9986295347545739443 ) ) ;
#1055 = DIRECTION ( 'NONE',  ( 1.000000000000000000, -1.291538348938060198E-32, 1.054621095516909827E-16 ) ) ;
#1056 = ORIENTED_EDGE ( 'NONE', *, *, #12207, .F. ) ;
#1057 = DIRECTION ( 'NONE',  ( -0.5691548339926012501, -0.8222303661035965661, 3.489949670251134954E-17 ) ) ;
#1058 = DIRECTION ( 'NONE',  ( 0.000000000000000000, -1.000000000000000000, -1.224646799147350002E-16 ) ) ;
#1059 = CARTESIAN_POINT ( 'NONE',  ( -15.49969986081092088, -13.50737899243822504, 57.00231026484397745 ) ) ;
#1060 = ORIENTED_EDGE ( 'NONE', *, *, #211, .F. ) ;
#1061 = DIRECTION ( 'NONE',  ( -0.9918751611018178371, -0.1272150336605033238, -7.193398003386547388E-16 ) ) ;
#1062 = ORIENTED_EDGE ( 'NONE', *, *, #6172, .F. ) ;
#1063 = LINE ( 'NONE', #4812, #9093 ) ;
#1064 = CARTESIAN_POINT ( 'NONE',  ( -18.09969986081099336, -109.6731500378498794, -10.30222923886191388 ) ) ;
#1065 = EDGE_CURVE ( 'NONE', #3619, #10638, #2411, .T. ) ;
#1066 = VECTOR ( 'NONE', #11148, 1000.000000000000114 ) ;
#1068 = CIRCLE ( 'NONE', #11320, 0.9999999999999990008 ) ;
#1067 = DIRECTION ( 'NONE',  ( -1.000000000000000000, 1.291538348938060198E-32, -1.054621095516909827E-16 ) ) ;
#1069 = DIRECTION ( 'NONE',  ( 8.018662683283438208E-16, -5.975035461963189015E-16, -1.000000000000000000 ) ) ;
#1070 = LINE ( 'NONE', #6640, #9198 ) ;
#1071 =( BOUNDED_CURVE ( )  B_SPLINE_CURVE ( 3, ( #5218, #486, #9882, #9806 ),
 .UNSPECIFIED., .F., .T. ) 
 B_SPLINE_CURVE_WITH_KNOTS ( ( 4, 4 ),
 ( 5.038118467679318258, 5.213043692789277372 ),
 .UNSPECIFIED. ) 
 CURVE ( )  GEOMETRIC_REPRESENTATION_ITEM ( )  RATIONAL_B_SPLINE_CURVE ( ( 1.000000000000000000, 0.9974517222217438306, 0.9974517222217438306, 1.000000000000000000 ) ) 
 REPRESENTATION_ITEM ( '' )  );
#1072 = CARTESIAN_POINT ( 'NONE',  ( -14.61203582816999891, -107.3496051183401647, -7.070526720097523921 ) ) ;
#1073 = DIRECTION ( 'NONE',  ( 0.5196486895212314439, -0.8543800322332368857, 9.271838545667882647E-16 ) ) ;
#1074 = CIRCLE ( 'NONE', #5710, 9.974999999999999645 ) ;
#1075 = CARTESIAN_POINT ( 'NONE',  ( -12.81093390292747713, -9.898980784960684787, 46.00231026484398456 ) ) ;
#1076 = ORIENTED_EDGE ( 'NONE', *, *, #13342, .T. ) ;
#1077 = CARTESIAN_POINT ( 'NONE',  ( 7.471063718837686274, 4.067408198524465668, 22.89737889731558340 ) ) ;
#1078 = ORIENTED_EDGE ( 'NONE', *, *, #8722, .T. ) ;
#1080 = ORIENTED_EDGE ( 'NONE', *, *, #198, .T. ) ;
#1079 = FACE_BOUND ( 'NONE', #11723, .T. ) ;
#1081 = EDGE_LOOP ( 'NONE', ( #9027, #14553, #6370, #10972 ) ) ;
#1082 = DIRECTION ( 'NONE',  ( -1.000000000000000000, 1.499759782661860071E-32, -1.224646799147350002E-16 ) ) ;
#1083 = VERTEX_POINT ( 'NONE', #11813 ) ;
#1084 = DIRECTION ( 'NONE',  ( 0.000000000000000000, 0.000000000000000000, 1.000000000000000000 ) ) ;
#1085 = EDGE_CURVE ( 'NONE', #13264, #8564, #9747, .T. ) ;
#1086 = CARTESIAN_POINT ( 'NONE',  ( -22.55857771067089246, -13.99059064457067336, 57.00231026484397745 ) ) ;
#1087 = VECTOR ( 'NONE', #14752, 1000.000000000000000 ) ;
#1088 = DIRECTION ( 'NONE',  ( -0.9085715390340232123, 0.4177292884839972631, -9.781476007338056784E-16 ) ) ;
#1089 = FACE_BOUND ( 'NONE', #8600, .T. ) ;
#1090 = ORIENTED_EDGE ( 'NONE', *, *, #13626, .T. ) ;
#1091 = CARTESIAN_POINT ( 'NONE',  ( 18.10099741743264445, -24.75028974787160507, 40.86364982085049036 ) ) ;
#1092 = VERTEX_POINT ( 'NONE', #5912 ) ;
#1093 = CARTESIAN_POINT ( 'NONE',  ( -1.508527451665001351, -44.77532818486911736, -5.497689735156003010 ) ) ;
#1094 = EDGE_LOOP ( 'NONE', ( #1225, #6586, #13232, #15058 ) ) ;
#1095 = ORIENTED_EDGE ( 'NONE', *, *, #8887, .F. ) ;
#1096 = STYLED_ITEM ( 'NONE', ( #2295 ), #7285 ) ;
#1097 = FACE_OUTER_BOUND ( 'NONE', #5270, .T. ) ;
#1098 = EDGE_LOOP ( 'NONE', ( #10426, #1549, #6086, #13428 ) ) ;
#1099 = CARTESIAN_POINT ( 'NONE',  ( -7.768926039458098565, -39.58069824233446354, 24.42899101494754888 ) ) ;
#1100 = ADVANCED_FACE ( 'NONE', ( #1337 ), #2635, .F. ) ;
#1101 = EDGE_CURVE ( 'NONE', #6582, #14153, #10860, .T. ) ;
#1102 = DIRECTION ( 'NONE',  ( 3.632077277826439854E-16, -1.000000000000000000, 0.000000000000000000 ) ) ;
#1103 = CARTESIAN_POINT ( 'NONE',  ( -10.12676381431746542, -90.53940471697117687, -5.497640657892870486 ) ) ;
#1104 = CARTESIAN_POINT ( 'NONE',  ( -15.49969986081099016, -36.50737899243799944, 27.50231026484399521 ) ) ;
#1106 = LINE ( 'NONE', #1413, #14279 ) ;
#1105 = DIRECTION ( 'NONE',  ( 0.000000000000000000, 0.1872998510044495413, 0.9823027872370673208 ) ) ;
#1107 = VERTEX_POINT ( 'NONE', #9441 ) ;
#1108 = CARTESIAN_POINT ( 'NONE',  ( -7.595066331666822990, -45.75350114379759958, 42.11098092323300790 ) ) ;
#1109 = DIRECTION ( 'NONE',  ( 0.000000000000000000, 1.131341397376178572E-16, -1.000000000000000000 ) ) ;
#1110 = ORIENTED_EDGE ( 'NONE', *, *, #4, .F. ) ;
#1111 = ORIENTED_EDGE ( 'NONE', *, *, #8455, .F. ) ;
#1112 = DIRECTION ( 'NONE',  ( 0.000000000000000000, 0.1872998510044759646, 0.9823027872370621028 ) ) ;
#1113 = CARTESIAN_POINT ( 'NONE',  ( -19.51357682882387934, -37.56763829276790290, -17.78480384862011832 ) ) ;
#1114 = CARTESIAN_POINT ( 'NONE',  ( -8.701256315749452241, -15.46758698257906950, 56.85231026484400019 ) ) ;
#1115 = ORIENTED_EDGE ( 'NONE', *, *, #13289, .T. ) ;
#1116 = CARTESIAN_POINT ( 'NONE',  ( -22.80943503306988873, -20.29474937510043375, 54.00231026484399166 ) ) ;
#1117 = EDGE_CURVE ( 'NONE', #8216, #15087, #8160, .T. ) ;
#1118 = EDGE_CURVE ( 'NONE', #13967, #642, #123, .T. ) ;
#1119 = AXIS2_PLACEMENT_3D ( 'NONE', #14284, #2727, #5103 ) ;
#1120 = CARTESIAN_POINT ( 'NONE',  ( -7.731023390221355207, -11.30308411758414877, 57.00231026484399166 ) ) ;
#1121 = EDGE_CURVE ( 'NONE', #9964, #7227, #3529, .T. ) ;
#1122 = CARTESIAN_POINT ( 'NONE',  ( -15.49969986081092088, -13.50737899243822504, 57.00231026484397745 ) ) ;
#1123 = CARTESIAN_POINT ( 'NONE',  ( -24.21370508435883906, -8.652820519829269585, 57.00231026484397745 ) ) ;
#1124 = ORIENTED_EDGE ( 'NONE', *, *, #3060, .F. ) ;
#1125 = CARTESIAN_POINT ( 'NONE',  ( -27.99969986081091733, -109.7258744763782943, -5.497689735156013668 ) ) ;
#1126 = CARTESIAN_POINT ( 'NONE',  ( -38.20013690429809827, 4.873818854045000037, 27.91208557747711083 ) ) ;
#1127 = CARTESIAN_POINT ( 'NONE',  ( -18.09969986081091875, -107.1622034095862972, -6.087689735156002868 ) ) ;
#1128 = DIRECTION ( 'NONE',  ( 0.000000000000000000, -1.000000000000000000, -1.224646799147350002E-16 ) ) ;
#1129 = ORIENTED_EDGE ( 'NONE', *, *, #13105, .F. ) ;
#1130 = CARTESIAN_POINT ( 'NONE',  ( -7.529934156977152959, -45.22371508067976720, 46.65625893024207471 ) ) ;
#1131 = ORIENTED_EDGE ( 'NONE', *, *, #12720, .F. ) ;
#1132 = CARTESIAN_POINT ( 'NONE',  ( -7.512805849530849400, -44.04964101872670312, 19.04457229113268113 ) ) ;
#1133 = CARTESIAN_POINT ( 'NONE',  ( -15.49969986081099904, -13.50737899243800122, 6.712064221500998684 ) ) ;
#1134 = EDGE_CURVE ( 'NONE', #13353, #11163, #4261, .T. ) ;
#1135 = DIRECTION ( 'NONE',  ( 0.000000000000000000, -1.000000000000000000, -1.224646799147350002E-16 ) ) ;
#1136 = AXIS2_PLACEMENT_3D ( 'NONE', #6177, #8477, #6325 ) ;
#1137 = CARTESIAN_POINT ( 'NONE',  ( -7.845610686729125760, -46.84038939242768151, 46.98533734250990790 ) ) ;
#1138 = CARTESIAN_POINT ( 'NONE',  ( -15.16333526000375187, -10.64029123852186132, 56.75231026484397745 ) ) ;
#1139 = DIRECTION ( 'NONE',  ( 0.5975035461963189576, 0.8018662683283437342, 0.000000000000000000 ) ) ;
#1140 = CARTESIAN_POINT ( 'NONE',  ( -20.62495262810510610, -107.5503273669732067, -7.108481602779681552 ) ) ;
#1141 = ADVANCED_FACE ( 'NONE', ( #8364 ), #8443, .T. ) ;
#1142 = CARTESIAN_POINT ( 'NONE',  ( -15.12053853660593283, -5.441285657357897598, 56.85231026484398598 ) ) ;
#1143 = VERTEX_POINT ( 'NONE', #11973 ) ;
#1144 = DIRECTION ( 'NONE',  ( 1.084202172485505026E-15, -0.1872998510044511788, -0.9823027872370668767 ) ) ;
#1145 = UNCERTAINTY_MEASURE_WITH_UNIT (LENGTH_MEASURE( 1.000000000000000082E-05 ), #14747, 'distance_accuracy_value', 'NONE');
#1146 = VERTEX_POINT ( 'NONE', #1489 ) ;
#1147 = CARTESIAN_POINT ( 'NONE',  ( -19.55678615628314532, -20.48959216528617233, 56.85231026484398598 ) ) ;
#1149 = ORIENTED_EDGE ( 'NONE', *, *, #12807, .F. ) ;
#1148 = FACE_OUTER_BOUND ( 'NONE', #8288, .T. ) ;
#1150 = VERTEX_POINT ( 'NONE', #10591 ) ;
#1151 = LINE ( 'NONE', #4836, #1160 ) ;
#1152 = ORIENTED_EDGE ( 'NONE', *, *, #4117, .T. ) ;
#1153 = VECTOR ( 'NONE', #6236, 999.9999999999998863 ) ;
#1154 = DIRECTION ( 'NONE',  ( -1.156482317317870344E-15, 1.000000000000000000, 0.000000000000000000 ) ) ;
#1155 = CARTESIAN_POINT ( 'NONE',  ( 7.000300139189000070, -19.50737899243799589, -5.787935778498998651 ) ) ;
#1156 = CARTESIAN_POINT ( 'NONE',  ( -7.512805849530849400, -44.04964101872670312, -5.955427708867301106 ) ) ;
#1157 = DIRECTION ( 'NONE',  ( 0.000000000000000000, 0.000000000000000000, 1.000000000000000000 ) ) ;
#1158 = VECTOR ( 'NONE', #12137, 999.9999999999998863 ) ;
#1159 = CARTESIAN_POINT ( 'NONE',  ( 17.56517143204546372, -24.02498291609396119, 6.519892126142639022 ) ) ;
#1160 = VECTOR ( 'NONE', #3603, 1000.000000000000000 ) ;
#1161 = CARTESIAN_POINT ( 'NONE',  ( -5.499699860811000818, -46.50737899243799944, 19.50231026484399877 ) ) ;
#1162 = EDGE_CURVE ( 'NONE', #12656, #14676, #12577, .T. ) ;
#1163 = DIRECTION ( 'NONE',  ( 0.000000000000000000, 0.000000000000000000, -1.000000000000000000 ) ) ;
#1164 = APPLICATION_CONTEXT ( 'automotive_design' ) ;
#1165 = VERTEX_POINT ( 'NONE', #10822 ) ;
#1166 = CARTESIAN_POINT ( 'NONE',  ( 3.909245658297777037, -38.51142663664874277, -12.58558199649565168 ) ) ;
#1167 = ORIENTED_EDGE ( 'NONE', *, *, #4732, .F. ) ;
#1168 = CARTESIAN_POINT ( 'NONE',  ( -15.49969986081091378, -13.50737899243822859, 51.00231026484399166 ) ) ;
#1169 = ORIENTED_EDGE ( 'NONE', *, *, #6172, .T. ) ;
#1170 = ORIENTED_EDGE ( 'NONE', *, *, #706, .T. ) ;
#1171 = LINE ( 'NONE', #1402, #14226 ) ;
#1172 = ORIENTED_EDGE ( 'NONE', *, *, #8951, .F. ) ;
#1173 = CONICAL_SURFACE ( 'NONE', #7510, 5.000000000000000000, 0.7853981633974476129 ) ;
#1174 = CONICAL_SURFACE ( 'NONE', #2147, 19.00000000000000000, 1.047197551196598297 ) ;
#1175 = CARTESIAN_POINT ( 'NONE',  ( -5.650856670168512785, -15.08880645082408556, 57.00231026484399166 ) ) ;
#1176 = VECTOR ( 'NONE', #6633, 1000.000000000000000 ) ;
#1177 = VECTOR ( 'NONE', #10955, 1000.000000000000227 ) ;
#1178 = CARTESIAN_POINT ( 'NONE',  ( -18.09969986081091520, -109.8057294739168981, -7.021413858388623197 ) ) ;
#1179 = CARTESIAN_POINT ( 'NONE',  ( -11.06942950089595712, -90.71429950798489017, -8.540436891703901523 ) ) ;
#1180 = DIRECTION ( 'NONE',  ( 1.000000000000000078E-15, -1.000000000000000000, 0.000000000000000000 ) ) ;
#1181 = ADVANCED_FACE ( 'NONE', ( #2709 ), #10664, .F. ) ;
#1183 = DIRECTION ( 'NONE',  ( 0.000000000000000000, 0.000000000000000000, 1.000000000000000000 ) ) ;
#1182 = CARTESIAN_POINT ( 'NONE',  ( 2.500300139188998738, -46.50737899243799944, 22.50231026484399877 ) ) ;
#1184 = AXIS2_PLACEMENT_3D ( 'NONE', #9205, #5615, #6752 ) ;
#1185 = ORIENTED_EDGE ( 'NONE', *, *, #4087, .T. ) ;
#1186 = CARTESIAN_POINT ( 'NONE',  ( -24.39712111458418775, -18.01698208283363556, 54.00231026484399166 ) ) ;
#1187 = DIRECTION ( 'NONE',  ( -0.5975035461963188466, -0.8018662683283439563, 0.000000000000000000 ) ) ;
#1188 = ORIENTED_EDGE ( 'NONE', *, *, #5624, .T. ) ;
#1189 = ORIENTED_EDGE ( 'NONE', *, *, #7592, .F. ) ;
#1190 = CARTESIAN_POINT ( 'NONE',  ( -7.064541492512758758, -18.83173137575486678, 54.00231026484400587 ) ) ;
#1191 = ADVANCED_FACE ( 'NONE', ( #13053 ), #10614, .T. ) ;
#1192 = DIRECTION ( 'NONE',  ( -8.018662683283438208E-16, 5.975035461963189015E-16, 1.000000000000000000 ) ) ;
#1193 = EDGE_LOOP ( 'NONE', ( #4642, #14603, #14008, #14703 ) ) ;
#1194 = SURFACE_STYLE_FILL_AREA ( #5924 ) ;
#1195 = ORIENTED_EDGE ( 'NONE', *, *, #11513, .T. ) ;
#1196 = AXIS2_PLACEMENT_3D ( 'NONE', #14185, #13126, #13050 ) ;
#1197 = CARTESIAN_POINT ( 'NONE',  ( -16.90917998795210053, -109.7162603717569311, -10.64494302517029212 ) ) ;
#1198 = CARTESIAN_POINT ( 'NONE',  ( -14.61203582817000068, -106.4047424672253186, -6.741402868119605429 ) ) ;
#1199 = CIRCLE ( 'NONE', #14634, 37.50000000000000000 ) ;
#1200 = LINE ( 'NONE', #13754, #10653 ) ;
#1201 = EDGE_CURVE ( 'NONE', #12600, #10787, #12478, .T. ) ;
#1202 = DIRECTION ( 'NONE',  ( 0.000000000000000000, -1.000000000000000000, -1.224646799147350002E-16 ) ) ;
#1203 = ORIENTED_EDGE ( 'NONE', *, *, #14579, .T. ) ;
#1204 = DIRECTION ( 'NONE',  ( 0.000000000000000000, 0.000000000000000000, 1.000000000000000000 ) ) ;
#1205 = LINE ( 'NONE', #4730, #9219 ) ;
#1206 = CARTESIAN_POINT ( 'NONE',  ( -15.49969986081099194, -27.00737899243800300, 11.50231026484399877 ) ) ;
#1207 = EDGE_CURVE ( 'NONE', #9069, #118, #5432, .T. ) ;
#1208 = LINE ( 'NONE', #3064, #4623 ) ;
#1209 = ORIENTED_EDGE ( 'NONE', *, *, #3266, .T. ) ;
#1210 = CARTESIAN_POINT ( 'NONE',  ( -7.502358996163085436, -44.29392756818862154, -6.675385003928089311 ) ) ;
#1211 = ORIENTED_EDGE ( 'NONE', *, *, #1496, .F. ) ;
#1212 = FACE_BOUND ( 'NONE', #878, .T. ) ;
#1213 = CARTESIAN_POINT ( 'NONE',  ( -15.49969986081099904, -2.007378992437998111, -3.787935778499002204 ) ) ;
#1214 = ADVANCED_FACE ( 'NONE', ( #7439 ), #9097, .F. ) ;
#1215 = CIRCLE ( 'NONE', #11469, 9.974999999999999645 ) ;
#1216 = CARTESIAN_POINT ( 'NONE',  ( -17.12834591918736749, -6.622385381944812188, 56.85231026484398598 ) ) ;
#1217 = SURFACE_SIDE_STYLE ('',( #13995 ) ) ;
#1218 = CARTESIAN_POINT ( 'NONE',  ( -18.86735971344653962, -5.080035572537331845, 57.00231026484397745 ) ) ;
#1219 = DIRECTION ( 'NONE',  ( 0.000000000000000000, 2.168404344971008868E-16, -1.000000000000000000 ) ) ;
#1220 = EDGE_CURVE ( 'NONE', #14257, #7843, #4288, .T. ) ;
#1221 = CARTESIAN_POINT ( 'NONE',  ( -33.49969986081099904, -42.00737899243800655, 52.39987856403599409 ) ) ;
#1222 = EDGE_CURVE ( 'NONE', #1625, #1508, #11426, .T. ) ;
#1223 = CARTESIAN_POINT ( 'NONE',  ( -35.26908782159542000, -38.19079675818825592, 51.36802084380344979 ) ) ;
#1224 = DIRECTION ( 'NONE',  ( 0.000000000000000000, -0.1872998510044521503, -0.9823027872370667657 ) ) ;
#1225 = ORIENTED_EDGE ( 'NONE', *, *, #14950, .T. ) ;
#1226 = DIRECTION ( 'NONE',  ( 0.5975035461963188466, 0.8018662683283437342, 0.000000000000000000 ) ) ;
#1227 = ORIENTED_EDGE ( 'NONE', *, *, #3624, .T. ) ;
#1229 = VERTEX_POINT ( 'NONE', #6489 ) ;
#1228 = CARTESIAN_POINT ( 'NONE',  ( -19.45253106704483770, -6.466019006254929202, 56.85231026484398598 ) ) ;
#1230 = ORIENTED_EDGE ( 'NONE', *, *, #13605, .F. ) ;
#1231 = CIRCLE ( 'NONE', #9782, 6.250000000000001776 ) ;
#1232 = CARTESIAN_POINT ( 'NONE',  ( -23.12048770254168062, -16.17743848078839619, 56.85231026484398598 ) ) ;
#1233 = ORIENTED_EDGE ( 'NONE', *, *, #9921, .T. ) ;
#1234 = CARTESIAN_POINT ( 'NONE',  ( -12.84854673063649599, -12.36513540471286809, 51.25231026484399166 ) ) ;
#1235 = DIRECTION ( 'NONE',  ( 1.000000000000000000, 0.000000000000000000, 1.011922027653137537E-15 ) ) ;
#1236 = CARTESIAN_POINT ( 'NONE',  ( -7.285742840713465007, -17.36641515085804599, 56.85231026484400019 ) ) ;
#1237 = SHAPE_REPRESENTATION_RELATIONSHIP ( 'NONE' , 'NONE' ,  #410, #6261 ) ;
#1238 = CARTESIAN_POINT ( 'NONE',  ( -20.87112600995948242, -85.00737899243800655, -5.497689735156005675 ) ) ;
#1239 = CYLINDRICAL_SURFACE ( 'NONE', #3766, 0.2500000000000004441 ) ;
#1240 = DIRECTION ( 'NONE',  ( -0.5975035461963188466, -0.8018662683283439563, 0.000000000000000000 ) ) ;
#1241 = ORIENTED_EDGE ( 'NONE', *, *, #13662, .T. ) ;
#1242 = CARTESIAN_POINT ( 'NONE',  ( 7.500300139189000070, -37.00737899243799944, -10.11609617439569675 ) ) ;
#1243 = VERTEX_POINT ( 'NONE', #2148 ) ;
#1244 = ORIENTED_EDGE ( 'NONE', *, *, #4054, .F. ) ;
#1245 = ORIENTED_EDGE ( 'NONE', *, *, #14708, .T. ) ;
#1246 = DIRECTION ( 'NONE',  ( 0.7276687409742212953, 0.6859287159822015090, 1.736481776669299976E-16 ) ) ;
#1247 = VERTEX_POINT ( 'NONE', #4441 ) ;
#1248 = AXIS2_PLACEMENT_3D ( 'NONE', #13525, #7691, #12375 ) ;
#1249 = CARTESIAN_POINT ( 'NONE',  ( 22.00030013918900096, -27.00737899243800300, 24.21206422150099868 ) ) ;
#1250 = EDGE_CURVE ( 'NONE', #1699, #13647, #7714, .T. ) ;
#1251 = FACE_OUTER_BOUND ( 'NONE', #10605, .T. ) ;
#1252 = CARTESIAN_POINT ( 'NONE',  ( -14.49553980497220174, -93.09698010465587004, -10.78611153367636888 ) ) ;
#1253 = AXIS2_PLACEMENT_3D ( 'NONE', #8330, #166, #9328 ) ;
#1254 = DIRECTION ( 'NONE',  ( 8.018662683283438208E-16, -5.975035461963189015E-16, -1.000000000000000000 ) ) ;
#1256 = CARTESIAN_POINT ( 'NONE',  ( -19.87664613915258371, -5.557310358991672139, 57.00231026484397745 ) ) ;
#1255 = CARTESIAN_POINT ( 'NONE',  ( -7.553613233656758297, -48.84439576093704716, -4.598074977179023470 ) ) ;
#1257 = ORIENTED_EDGE ( 'NONE', *, *, #7736, .F. ) ;
#1258 = FACE_OUTER_BOUND ( 'NONE', #72, .T. ) ;
#1259 = CARTESIAN_POINT ( 'NONE',  ( -19.97045281939299954, -14.09771657249876142, -13.02052492037858933 ) ) ;
#1260 = VERTEX_POINT ( 'NONE', #10017 ) ;
#1261 = ORIENTED_EDGE ( 'NONE', *, *, #492, .F. ) ;
#1262 = CARTESIAN_POINT ( 'NONE',  ( 21.99148493447345132, -30.15430098416778648, 25.05124702636123146 ) ) ;
#1263 = CARTESIAN_POINT ( 'NONE',  ( -19.73154169590003093, -37.71326103272679120, 56.76340952534463469 ) ) ;
#1264 = EDGE_LOOP ( 'NONE', ( #4426, #9254, #14569, #1426 ) ) ;
#1265 =( NAMED_UNIT ( * ) PLANE_ANGLE_UNIT ( ) SI_UNIT ( $, .RADIAN. ) );
#1266 = VERTEX_POINT ( 'NONE', #5653 ) ;
#1267 = CIRCLE ( 'NONE', #2254, 37.50000000000000000 ) ;
#1268 = VECTOR ( 'NONE', #9947, 1000.000000000000000 ) ;
#1269 = ADVANCED_FACE ( 'NONE', ( #12632 ), #4370, .F. ) ;
#1270 = CARTESIAN_POINT ( 'NONE',  ( -17.61203582817000424, -106.8344286703292028, -4.368659857491135945 ) ) ;
#1271 = LINE ( 'NONE', #10840, #12360 ) ;
#1272 = PLANE ( 'NONE',  #15007 ) ;
#1273 = VECTOR ( 'NONE', #11597, 1000.000000000000114 ) ;
#1274 = ORIENTED_EDGE ( 'NONE', *, *, #14320, .F. ) ;
#1275 = CARTESIAN_POINT ( 'NONE',  ( -17.72286745096104355, -3.783277446994212312, 54.00231026484397745 ) ) ;
#1276 = AXIS2_PLACEMENT_3D ( 'NONE', #1608, #11091, #13328 ) ;
#1277 = LINE ( 'NONE', #5937, #679 ) ;
#1278 = ORIENTED_EDGE ( 'NONE', *, *, #13298, .T. ) ;
#1279 = VECTOR ( 'NONE', #13433, 1000.000000000000000 ) ;
#1280 = AXIS2_PLACEMENT_3D ( 'NONE', #7638, #12245, #11247 ) ;
#1281 = DIRECTION ( 'NONE',  ( 0.000000000000000000, 1.224646799147350002E-16, -1.000000000000000000 ) ) ;
#1282 = EDGE_LOOP ( 'NONE', ( #9084, #8815, #10468, #11123, #3395 ) ) ;
#1283 = DIRECTION ( 'NONE',  ( -0.02283895005206026604, 0.9997391571607663341, -6.156614753256598861E-16 ) ) ;
#1284 = ORIENTED_EDGE ( 'NONE', *, *, #14044, .T. ) ;
#1285 = CARTESIAN_POINT ( 'NONE',  ( -7.425287632467987287, -13.60480674405941492, 56.85231026484400019 ) ) ;
#1286 = CARTESIAN_POINT ( 'NONE',  ( 6.045543233663400073, 3.992621007561997892, 24.26206422150100295 ) ) ;
#1287 = CARTESIAN_POINT ( 'NONE',  ( -22.04595456446742929, -18.23578246029658345, 56.85231026484398598 ) ) ;
#1288 = ADVANCED_FACE ( 'NONE', ( #4217 ), #8871, .T. ) ;
#1289 = LINE ( 'NONE', #9629, #10065 ) ;
#1290 = DIRECTION ( 'NONE',  ( 0.000000000000000000, -0.9895257890689694857, 0.1443562010009729335 ) ) ;
#1291 = VECTOR ( 'NONE', #13358, 1000.000000000000000 ) ;
#1292 = VECTOR ( 'NONE', #13779, 1000.000000000000114 ) ;
#1293 = EDGE_CURVE ( 'NONE', #2996, #2185, #9966, .T. ) ;
#1294 = CARTESIAN_POINT ( 'NONE',  ( -6.519606984562681617, -17.91311303219895024, 60.62118659065755111 ) ) ;
#1295 = FACE_OUTER_BOUND ( 'NONE', #14589, .T. ) ;
#1296 = ORIENTED_EDGE ( 'NONE', *, *, #7957, .T. ) ;
#1297 = CARTESIAN_POINT ( 'NONE',  ( -15.49969986081099904, -44.50737899243799944, -109.5506571639849938 ) ) ;
#1298 = LINE ( 'NONE', #8326, #6779 ) ;
#1299 = LINE ( 'NONE', #4670, #10833 ) ;
#1300 = ORIENTED_EDGE ( 'NONE', *, *, #5722, .T. ) ;
#1301 = PLANE ( 'NONE',  #14942 ) ;
#1302 = PRODUCT_DEFINITION_CONTEXT ( 'detailed design', #107, 'design' ) ;
#1303 = ORIENTED_EDGE ( 'NONE', *, *, #10829, .T. ) ;
#1304 = ADVANCED_FACE ( 'NONE', ( #13776 ), #6715, .F. ) ;
#1306 = ORIENTED_EDGE ( 'NONE', *, *, #5188, .T. ) ;
#1305 = FACE_OUTER_BOUND ( 'NONE', #8694, .T. ) ;
#1307 = B_SPLINE_CURVE_WITH_KNOTS ( 'NONE', 3,
 ( #7540, #663, #8621, #14437, #14587, #6462, #594, #13306, #1891, #1661, #2882, #3106, #7465, #12142, #10993, #4182, #12220, #6313, #5109, #516, #6538, #742, #1731, #8765, #8836, #4036, #5176, #7765, #5256, #14516, #9848, #1816, #8689, #13371 ),
 .UNSPECIFIED., .F., .F.,
 ( 4, 2, 2, 2, 2, 2, 2, 2, 2, 2, 2, 2, 2, 2, 2, 2, 4 ),
 ( 0.01024809238176392634, 0.01088874702714459804, 0.01152940167252526973, 0.01217005631790594143, 0.01281071096328661313, 0.01345136560866728656, 0.01409202025404795826, 0.01473267489942862996, 0.01537332954480930165, 0.01601398419018997335, 0.01665463883557064678, 0.01729529348095131674, 0.01793594812633199018, 0.01857660277171266361, 0.01921725741709333357, 0.01985791206247400353, 0.02049856670785467697 ),
 .UNSPECIFIED. ) ;
#1308 = VERTEX_POINT ( 'NONE', #8943 ) ;
#1309 = CIRCLE ( 'NONE', #335, 0.4500000000000011768 ) ;
#1310 = DIRECTION ( 'NONE',  ( 0.8018662683283436232, -0.5975035461963189576, 9.999999999999996833E-16 ) ) ;
#1311 = ORIENTED_EDGE ( 'NONE', *, *, #9300, .T. ) ;
#1312 = AXIS2_PLACEMENT_3D ( 'NONE', #13815, #9136, #1109 ) ;
#1313 = CARTESIAN_POINT ( 'NONE',  ( -23.36093307149983289, -11.66014798166512634, 57.00231026484397745 ) ) ;
#1314 = EDGE_CURVE ( 'NONE', #11680, #6476, #3622, .T. ) ;
#1315 = EDGE_CURVE ( 'NONE', #10582, #1699, #3140, .T. ) ;
#1316 = LINE ( 'NONE', #8419, #6466 ) ;
#1317 = EDGE_CURVE ( 'NONE', #3567, #2643, #6642, .T. ) ;
#1318 = CARTESIAN_POINT ( 'NONE',  ( -21.67659902633306146, -21.33978230808610022, 56.85231026484398598 ) ) ;
#1319 = DIRECTION ( 'NONE',  ( 1.000000000000000000, 0.000000000000000000, 0.000000000000000000 ) ) ;
#1320 = CARTESIAN_POINT ( 'NONE',  ( -18.15085299098534222, -14.64962258016358732, 56.89875687425072215 ) ) ;
#1321 = CIRCLE ( 'NONE', #5461, 0.4500000000000011768 ) ;
#1322 = DIRECTION ( 'NONE',  ( 0.000000000000000000, 0.000000000000000000, 1.000000000000000000 ) ) ;
#1323 = FACE_OUTER_BOUND ( 'NONE', #14535, .T. ) ;
#1324 = CARTESIAN_POINT ( 'NONE',  ( -11.92171335822600042, -16.25216409852338373, -13.11721111237203630 ) ) ;
#1325 = VERTEX_POINT ( 'NONE', #5577 ) ;
#1326 = CARTESIAN_POINT ( 'NONE',  ( -15.09158957740191731, -107.1622034095870077, -6.087689735156000204 ) ) ;
#1327 = VECTOR ( 'NONE', #6528, 1000.000000000000000 ) ;
#1328 = ORIENTED_EDGE ( 'NONE', *, *, #3030, .T. ) ;
#1329 = ORIENTED_EDGE ( 'NONE', *, *, #11138, .T. ) ;
#1330 = DIRECTION ( 'NONE',  ( -8.018662683283438208E-16, 5.975035461963189015E-16, 1.000000000000000000 ) ) ;
#1331 = ORIENTED_EDGE ( 'NONE', *, *, #3928, .F. ) ;
#1332 = CARTESIAN_POINT ( 'NONE',  ( -10.84210729886283531, -6.910555398701176522, 57.00231026484397745 ) ) ;
#1333 = VECTOR ( 'NONE', #8633, 1000.000000000000000 ) ;
#1334 = EDGE_CURVE ( 'NONE', #14079, #470, #10249, .T. ) ;
#1335 = CARTESIAN_POINT ( 'NONE',  ( -7.512805849530849400, -44.04964101872670312, -5.955427708867301106 ) ) ;
#1336 = CARTESIAN_POINT ( 'NONE',  ( -11.85919799147835363, -90.99634588947422742, -9.447245264708476142 ) ) ;
#1337 = FACE_OUTER_BOUND ( 'NONE', #4258, .T. ) ;
#1338 = AXIS2_PLACEMENT_3D ( 'NONE', #7490, #12099, #1610 ) ;
#1340 = CARTESIAN_POINT ( 'NONE',  ( -15.49969986081099904, 64.39262100756199914, 24.21206422150100579 ) ) ;
#1339 = CARTESIAN_POINT ( 'NONE',  ( -7.508350897672356972, -44.16519039693573490, 20.39701027657645227 ) ) ;
#1341 = ORIENTED_EDGE ( 'NONE', *, *, #13293, .F. ) ;
#1342 = DIRECTION ( 'NONE',  ( 9.804908406240741039E-16, -0.05233595624294555548, -0.9986295347545738332 ) ) ;
#1343 = CARTESIAN_POINT ( 'NONE',  ( -24.47770327408855806, -17.91589678518842277, 60.62170142699616804 ) ) ;
#1344 = ORIENTED_EDGE ( 'NONE', *, *, #13456, .T. ) ;
#1345 = ORIENTED_EDGE ( 'NONE', *, *, #2264, .F. ) ;
#1346 = CARTESIAN_POINT ( 'NONE',  ( 21.94844983914712344, -29.59392153401264380, 26.19129280141764937 ) ) ;
#1347 = ADVANCED_FACE ( 'NONE', ( #3932 ), #13278, .T. ) ;
#1348 = CARTESIAN_POINT ( 'NONE',  ( -15.49969986081099904, -52.50737899243799944, 57.00231026484399166 ) ) ;
#1349 = VERTEX_POINT ( 'NONE', #1375 ) ;
#1350 = DIRECTION ( 'NONE',  ( -0.9983330752162417054, -0.05771543059946733500, -7.660444431189781397E-16 ) ) ;
#1351 = VECTOR ( 'NONE', #1366, 1000.000000000000000 ) ;
#1352 = PLANE ( 'NONE',  #3170 ) ;
#1353 = CARTESIAN_POINT ( 'NONE',  ( -14.61203582817000068, -107.9196643519486827, -5.433976602192393202 ) ) ;
#1354 = PLANE ( 'NONE',  #15041 ) ;
#1355 = PLANE ( 'NONE',  #3232 ) ;
#1356 = VERTEX_POINT ( 'NONE', #3594 ) ;
#1357 = CARTESIAN_POINT ( 'NONE',  ( -12.38873450203231030, -7.152605626181999909, 56.85231026484398598 ) ) ;
#1358 = DIRECTION ( 'NONE',  ( 0.000000000000000000, 0.000000000000000000, -1.000000000000000000 ) ) ;
#1359 = ORIENTED_EDGE ( 'NONE', *, *, #6811, .T. ) ;
#1360 = ADVANCED_FACE ( 'NONE', ( #7094 ), #4521, .F. ) ;
#1361 = DIRECTION ( 'NONE',  ( -8.018662683283438208E-16, 5.975035461963189015E-16, 1.000000000000000000 ) ) ;
#1362 = ORIENTED_EDGE ( 'NONE', *, *, #12175, .T. ) ;
#1363 = LINE ( 'NONE', #8314, #10601 ) ;
#1364 = ORIENTED_EDGE ( 'NONE', *, *, #8217, .F. ) ;
#1365 = DIRECTION ( 'NONE',  ( 0.000000000000000000, 1.000000000000000000, 1.224646799147350002E-16 ) ) ;
#1366 = DIRECTION ( 'NONE',  ( 8.018662683283438208E-16, -5.975035461963189015E-16, -1.000000000000000000 ) ) ;
#1367 = DIRECTION ( 'NONE',  ( 0.000000000000000000, -1.000000000000000000, -1.224646799147350002E-16 ) ) ;
#1368 = FILL_AREA_STYLE ('',( #14149 ) ) ;
#1369 = EDGE_CURVE ( 'NONE', #7843, #12569, #3122, .T. ) ;
#1370 = CARTESIAN_POINT ( 'NONE',  ( -9.251715890255169938, -8.391880844292892050, 57.00231026484397745 ) ) ;
#1371 = VECTOR ( 'NONE', #14303, 1000.000000000000000 ) ;
#1372 = LINE ( 'NONE', #14229, #10895 ) ;
#1373 = ORIENTED_EDGE ( 'NONE', *, *, #8795, .T. ) ;
#1374 = DIRECTION ( 'NONE',  ( -8.018662683283438208E-16, 5.975035461963189015E-16, 1.000000000000000000 ) ) ;
#1375 = CARTESIAN_POINT ( 'NONE',  ( -7.480766807389218620, -12.55450823271226746, 57.00231026484399166 ) ) ;
#1376 = CARTESIAN_POINT ( 'NONE',  ( -3.508527451665000463, -45.20834088676133433, -6.247689735156000346 ) ) ;
#1377 = EDGE_CURVE ( 'NONE', #1475, #9010, #11552, .T. ) ;
#1378 = VERTEX_POINT ( 'NONE', #84 ) ;
#1379 = CARTESIAN_POINT ( 'NONE',  ( 7.246718728573819490, 4.729174316162667147, 20.79414966637559914 ) ) ;
#1380 = VERTEX_POINT ( 'NONE', #3370 ) ;
#1381 = ORIENTED_EDGE ( 'NONE', *, *, #12726, .T. ) ;
#1382 = EDGE_LOOP ( 'NONE', ( #10001, #11400, #3067, #7270 ) ) ;
#1383 = EDGE_CURVE ( 'NONE', #7657, #9919, #8251, .T. ) ;
#1384 = DIRECTION ( 'NONE',  ( 8.018662683283438208E-16, -5.975035461963189015E-16, -1.000000000000000000 ) ) ;
#1385 = VERTEX_POINT ( 'NONE', #14075 ) ;
#1386 =( BOUNDED_CURVE ( )  B_SPLINE_CURVE ( 3, ( #8741, #2858, #5089, #6442 ),
 .UNSPECIFIED., .F., .T. ) 
 B_SPLINE_CURVE_WITH_KNOTS ( ( 4, 4 ),
 ( 5.789511490773299407, 7.299387194767466447 ),
 .UNSPECIFIED. ) 
 CURVE ( )  GEOMETRIC_REPRESENTATION_ITEM ( )  RATIONAL_B_SPLINE_CURVE ( ( 1.000000000000000000, 0.8188760873989396893, 0.8188760873989396893, 1.000000000000000000 ) ) 
 REPRESENTATION_ITEM ( '' )  );
#1387 = FACE_OUTER_BOUND ( 'NONE', #203, .T. ) ;
#1388 = CARTESIAN_POINT ( 'NONE',  ( -33.43612459436373996, 11.05255549926123493, 16.20867245922678990 ) ) ;
#1389 = DIRECTION ( 'NONE',  ( 0.000000000000000000, -1.000000000000000000, -1.224646799147350002E-16 ) ) ;
#1391 = B_SPLINE_CURVE_WITH_KNOTS ( 'NONE', 3,
 ( #11818, #7214, #9599, #1343, #5994, #10901, #9521, #3940, #7295, #2791, #429, #2716 ),
 .UNSPECIFIED., .F., .F.,
 ( 4, 2, 2, 2, 2, 4 ),
 ( 0.000000000000000000, 0.03633466677368843434, 0.05450200016053259600, 0.07266933354737674378, 0.1090040003210653030, 0.1453386670947538206 ),
 .UNSPECIFIED. ) ;
#1390 = LINE ( 'NONE', #14017, #1912 ) ;
#1392 = AXIS2_PLACEMENT_3D ( 'NONE', #13825, #830, #8925 ) ;
#1393 = CARTESIAN_POINT ( 'NONE',  ( 22.00030013918900096, -27.00737899243800300, 43.21206422150100224 ) ) ;
#1394 = EDGE_CURVE ( 'NONE', #11477, #118, #11776, .T. ) ;
#1395 = CARTESIAN_POINT ( 'NONE',  ( 4.180649471280372786, -38.26834254388227663, -12.41843850008141992 ) ) ;
#1396 = EDGE_CURVE ( 'NONE', #5861, #745, #8020, .T. ) ;
#1397 = ORIENTED_EDGE ( 'NONE', *, *, #15002, .F. ) ;
#1398 = ORIENTED_EDGE ( 'NONE', *, *, #6504, .F. ) ;
#1399 = AXIS2_PLACEMENT_3D ( 'NONE', #1868, #13648, #1714 ) ;
#1400 = VERTEX_POINT ( 'NONE', #10400 ) ;
#1401 = EDGE_CURVE ( 'NONE', #10974, #3638, #5757, .T. ) ;
#1402 = CARTESIAN_POINT ( 'NONE',  ( -22.54723635769173384, -9.564857042577559199, 56.85231026484398598 ) ) ;
#1403 = ORIENTED_EDGE ( 'NONE', *, *, #11594, .F. ) ;
#1404 = DIRECTION ( 'NONE',  ( -8.018662683283438208E-16, 5.975035461963189015E-16, 1.000000000000000000 ) ) ;
#1405 = LINE ( 'NONE', #3849, #8849 ) ;
#1406 = AXIS2_PLACEMENT_3D ( 'NONE', #13534, #8929, #5266 ) ;
#1407 = EDGE_CURVE ( 'NONE', #2678, #8358, #1298, .T. ) ;
#1408 = CARTESIAN_POINT ( 'NONE',  ( -14.07534335717186202, -5.558639560896826204, 56.85231026484398598 ) ) ;
#1409 = CIRCLE ( 'NONE', #4101, 9.974999999999999645 ) ;
#1410 = LINE ( 'NONE', #6059, #7036 ) ;
#1411 = DIRECTION ( 'NONE',  ( -8.018662683283438208E-16, 5.975035461963189015E-16, 1.000000000000000000 ) ) ;
#1413 = CARTESIAN_POINT ( 'NONE',  ( -8.667632128016617088, -19.48099602858229318, 57.00231026484399166 ) ) ;
#1412 = CARTESIAN_POINT ( 'NONE',  ( -7.503901077028577227, -48.99487332462116740, -5.755859045742772295 ) ) ;
#1414 = EDGE_CURVE ( 'NONE', #855, #11014, #5593, .T. ) ;
#1415 = ORIENTED_EDGE ( 'NONE', *, *, #4203, .T. ) ;
#1416 = CARTESIAN_POINT ( 'NONE',  ( -15.49969986081092088, -13.50737899243822504, 56.85231026484398598 ) ) ;
#1417 = EDGE_CURVE ( 'NONE', #3424, #6799, #8006, .T. ) ;
#1418 = AXIS2_PLACEMENT_3D ( 'NONE', #10149, #14679, #8781 ) ;
#1419 = AXIS2_PLACEMENT_3D ( 'NONE', #5617, #10131, #3181 ) ;
#1420 = CARTESIAN_POINT ( 'NONE',  ( -8.791486474964735010, -6.124933722071896014, 57.00231026484397745 ) ) ;
#1421 = ORIENTED_EDGE ( 'NONE', *, *, #8034, .T. ) ;
#1422 = ORIENTED_EDGE ( 'NONE', *, *, #7827, .T. ) ;
#1423 = CARTESIAN_POINT ( 'NONE',  ( 21.98624202466326238, -30.09200759101065614, 25.25752346147605820 ) ) ;
#1424 = AXIS2_PLACEMENT_3D ( 'NONE', #4250, #12289, #2950 ) ;
#1425 = CARTESIAN_POINT ( 'NONE',  ( -11.30335942247960190, -22.55676305576680818, 54.00231026484399166 ) ) ;
#1426 = ORIENTED_EDGE ( 'NONE', *, *, #3675, .T. ) ;
#1427 = FILL_AREA_STYLE_COLOUR ( '', #13311 ) ;
#1428 = FACE_OUTER_BOUND ( 'NONE', #3168, .T. ) ;
#1429 = B_SPLINE_CURVE_WITH_KNOTS ( 'NONE', 3,
 ( #4750, #1379, #7098, #10712, #3678, #1077, #5878, #9561 ),
 .UNSPECIFIED., .F., .F.,
 ( 4, 2, 2, 4 ),
 ( 0.000000000000000000, 0.2499999999999993894, 0.4999999999999987788, 1.000000000000000000 ),
 .UNSPECIFIED. ) ;
#1430 = EDGE_CURVE ( 'NONE', #3542, #8123, #8406, .T. ) ;
#1431 = CARTESIAN_POINT ( 'NONE',  ( -7.499699860810999041, -19.50737899243799589, 56.13904046828879757 ) ) ;
#1432 = AXIS2_PLACEMENT_3D ( 'NONE', #9239, #3665, #8319 ) ;
#1433 = DIRECTION ( 'NONE',  ( -8.018662683283439195E-16, 5.975035461963190001E-16, 1.000000000000000000 ) ) ;
#1434 = CARTESIAN_POINT ( 'NONE',  ( -23.49969986081099194, -49.19367049345326137, 24.18860176585926425 ) ) ;
#1435 = EDGE_LOOP ( 'NONE', ( #12352, #4053, #12715, #5829, #11865, #12279, #4757 ) ) ;
#1436 = PLANE ( 'NONE',  #6755 ) ;
#1437 = FACE_OUTER_BOUND ( 'NONE', #183, .T. ) ;
#1438 = ORIENTED_EDGE ( 'NONE', *, *, #11015, .F. ) ;
#1439 = CARTESIAN_POINT ( 'NONE',  ( -7.508318444979633632, -44.14098664639713832, 18.67373629545663150 ) ) ;
#1440 = DIRECTION ( 'NONE',  ( -8.018662683283439195E-16, 5.975035461963190001E-16, 1.000000000000000000 ) ) ;
#1441 = ORIENTED_EDGE ( 'NONE', *, *, #7113, .T. ) ;
#1442 = CARTESIAN_POINT ( 'NONE',  ( -23.49969986081099904, -44.50737899243799944, 19.50231026484399877 ) ) ;
#1443 = ORIENTED_EDGE ( 'NONE', *, *, #5114, .T. ) ;
#1444 = CARTESIAN_POINT ( 'NONE',  ( -15.49969986081099194, -57.00737899243800655, 11.50231026484399521 ) ) ;
#1445 = FACE_OUTER_BOUND ( 'NONE', #274, .T. ) ;
#1446 = VECTOR ( 'NONE', #6854, 1000.000000000000000 ) ;
#1447 = EDGE_CURVE ( 'NONE', #7867, #5848, #5803, .T. ) ;
#1448 = ADVANCED_FACE ( 'NONE', ( #1453 ), #1173, .T. ) ;
#1449 = FACE_OUTER_BOUND ( 'NONE', #11049, .T. ) ;
#1450 = CARTESIAN_POINT ( 'NONE',  ( 17.25070158960591016, -30.18020639231665925, 5.944247395788684329 ) ) ;
#1451 = VERTEX_POINT ( 'NONE', #9863 ) ;
#1452 = CARTESIAN_POINT ( 'NONE',  ( -8.313210069164949090, -48.06114224692424841, -17.30321196480585400 ) ) ;
#1453 = FACE_OUTER_BOUND ( 'NONE', #7463, .T. ) ;
#1454 = PLANE ( 'NONE',  #7150 ) ;
#1455 = VERTEX_POINT ( 'NONE', #13243 ) ;
#1456 = CARTESIAN_POINT ( 'NONE',  ( -7.508347634011948379, -44.16528234937342035, -4.602730171981503915 ) ) ;
#1457 = AXIS2_PLACEMENT_3D ( 'NONE', #10103, #4303, #8956 ) ;
#1458 = ORIENTED_EDGE ( 'NONE', *, *, #8209, .T. ) ;
#1460 = VERTEX_POINT ( 'NONE', #14530 ) ;
#1459 = FACE_OUTER_BOUND ( 'NONE', #4180, .T. ) ;
#1461 = ORIENTED_EDGE ( 'NONE', *, *, #1671, .T. ) ;
#1462 = VECTOR ( 'NONE', #2494, 1000.000000000000000 ) ;
#1463 = DIRECTION ( 'NONE',  ( -0.3533329742249643468, -0.9354976265738683683, 2.756373558169988451E-16 ) ) ;
#1464 = EDGE_LOOP ( 'NONE', ( #6842, #9273, #8453, #1056 ) ) ;
#1465 = CARTESIAN_POINT ( 'NONE',  ( -7.754930580632606762, -46.50765881518451295, 22.00225574842814424 ) ) ;
#1466 = EDGE_CURVE ( 'NONE', #2901, #8324, #6287, .T. ) ;
#1467 = DIRECTION ( 'NONE',  ( 0.5975035461963188466, 0.8018662683283437342, 0.000000000000000000 ) ) ;
#1468 = DIRECTION ( 'NONE',  ( 0.000000000000000000, 0.000000000000000000, 1.000000000000000000 ) ) ;
#1469 = CARTESIAN_POINT ( 'NONE',  ( 18.35447865076064744, -25.46704448935311760, 8.082739883746024034 ) ) ;
#1470 = DIRECTION ( 'NONE',  ( -0.02283895005205794151, 0.9997391571607663341, -6.156614753256579139E-16 ) ) ;
#1471 = CARTESIAN_POINT ( 'NONE',  ( -15.61203582817000068, -106.5081018427098201, -6.912624477443467974 ) ) ;
#1472 = ORIENTED_EDGE ( 'NONE', *, *, #4194, .T. ) ;
#1473 = CARTESIAN_POINT ( 'NONE',  ( -13.24180272517058654, -17.41093464048234551, -13.22069529846239888 ) ) ;
#1474 = COLOUR_RGB ( '', 0.09019608, 0.27058824, 0.51372549) ;
#1475 = VERTEX_POINT ( 'NONE', #8636 ) ;
#1476 =( BOUNDED_CURVE ( )  B_SPLINE_CURVE ( 3, ( #1533, #8487, #10714, #242 ),
 .UNSPECIFIED., .F., .T. ) 
 B_SPLINE_CURVE_WITH_KNOTS ( ( 4, 4 ),
 ( -8.881784197001252323E-16, 1.570796326794895670 ),
 .UNSPECIFIED. ) 
 CURVE ( )  GEOMETRIC_REPRESENTATION_ITEM ( )  RATIONAL_B_SPLINE_CURVE ( ( 1.000000000000000000, 0.8047378541243649375, 0.8047378541243649375, 1.000000000000000000 ) ) 
 REPRESENTATION_ITEM ( '' )  );
#1477 = LINE ( 'NONE', #13191, #12443 ) ;
#1478 = ORIENTED_EDGE ( 'NONE', *, *, #10848, .F. ) ;
#1479 = ORIENTED_EDGE ( 'NONE', *, *, #3283, .T. ) ;
#1480 = CARTESIAN_POINT ( 'NONE',  ( 6.906785209640905698, -37.00737899243799944, 49.58160724549794196 ) ) ;
#1481 = ORIENTED_EDGE ( 'NONE', *, *, #1803, .T. ) ;
#1482 = CARTESIAN_POINT ( 'NONE',  ( -8.681233859935403530, -6.226640953275949464, 54.00231026484399166 ) ) ;
#1483 = CARTESIAN_POINT ( 'NONE',  ( -6.424455519809837867, -13.54187755947681993, 56.85231026484400019 ) ) ;
#1484 = EDGE_CURVE ( 'NONE', #3312, #4359, #4097, .T. ) ;
#1485 = SURFACE_SIDE_STYLE ('',( #12972 ) ) ;
#1486 = CARTESIAN_POINT ( 'NONE',  ( -12.20995213488984277, -91.16154615634617642, -9.744773464311498046 ) ) ;
#1487 = CIRCLE ( 'NONE', #9294, 15.87500000000000355 ) ;
#1488 = EDGE_CURVE ( 'NONE', #5098, #9431, #6331, .T. ) ;
#1489 = CARTESIAN_POINT ( 'NONE',  ( -19.27841348868324545, -22.73895244004356897, 56.85231026484400019 ) ) ;
#1491 = DIRECTION ( 'NONE',  ( -8.018662683283438208E-16, 5.975035461963189015E-16, 1.000000000000000000 ) ) ;
#1490 = CARTESIAN_POINT ( 'NONE',  ( -7.705418609684434372, -48.24386234041418220, -3.676323684936692260 ) ) ;
#1492 = ORIENTED_EDGE ( 'NONE', *, *, #6404, .T. ) ;
#1493 = CARTESIAN_POINT ( 'NONE',  ( -7.501944906337848273, -44.50613385756380325, -4.001965388595783324 ) ) ;
#1494 = CARTESIAN_POINT ( 'NONE',  ( -34.99969986081099904, -20.37340439622244048, 51.53354502093799994 ) ) ;
#1495 = VERTEX_POINT ( 'NONE', #8482 ) ;
#1496 = EDGE_CURVE ( 'NONE', #11960, #951, #7556, .T. ) ;
#1497 = EDGE_LOOP ( 'NONE', ( #9660, #8651, #10886, #469 ) ) ;
#1498 = DIRECTION ( 'NONE',  ( 0.7276687409742212953, 0.6859287159822015090, 1.736481776669299976E-16 ) ) ;
#1499 = ORIENTED_EDGE ( 'NONE', *, *, #15040, .F. ) ;
#1500 = CYLINDRICAL_SURFACE ( 'NONE', #1570, 3.249999999999999556 ) ;
#1501 = EDGE_CURVE ( 'NONE', #2831, #10753, #529, .T. ) ;
#1502 = DIRECTION ( 'NONE',  ( -1.000000000000000000, 1.291538348938060198E-32, -1.054621095516909827E-16 ) ) ;
#1503 = EDGE_CURVE ( 'NONE', #7413, #9431, #12902, .T. ) ;
#1504 = AXIS2_PLACEMENT_3D ( 'NONE', #14260, #6843, #10451 ) ;
#1505 = CARTESIAN_POINT ( 'NONE',  ( -11.14685911689329245, -22.51056837233514329, 56.74883337938142347 ) ) ;
#1506 = LINE ( 'NONE', #13300, #2350 ) ;
#1507 = CARTESIAN_POINT ( 'NONE',  ( -20.18599136182622544, -52.50737899243804918, 27.50231026484403429 ) ) ;
#1508 = VERTEX_POINT ( 'NONE', #9711 ) ;
#1509 = CARTESIAN_POINT ( 'NONE',  ( -15.49969986081095996, -67.00737899243799234, -5.497689735156000346 ) ) ;
#1510 = PLANE ( 'NONE',  #3630 ) ;
#1511 = ORIENTED_EDGE ( 'NONE', *, *, #2712, .F. ) ;
#1512 = VECTOR ( 'NONE', #8602, 1000.000000000000227 ) ;
#1513 = CARTESIAN_POINT ( 'NONE',  ( -15.61203582817000068, -106.2504437127206529, -5.561324420954690595 ) ) ;
#1514 = ORIENTED_EDGE ( 'NONE', *, *, #942, .T. ) ;
#1515 = DIRECTION ( 'NONE',  ( -1.000000000000000000, 0.000000000000000000, 0.000000000000000000 ) ) ;
#1516 = VERTEX_POINT ( 'NONE', #5194 ) ;
#1517 = DIRECTION ( 'NONE',  ( 8.018662683283438208E-16, -5.975035461963189015E-16, -1.000000000000000000 ) ) ;
#1518 = CIRCLE ( 'NONE', #1024, 19.00000000000000000 ) ;
#1519 = FACE_OUTER_BOUND ( 'NONE', #6294, .T. ) ;
#1520 = CARTESIAN_POINT ( 'NONE',  ( -15.49969986081099904, -36.50737899243799944, -13.49768973515600479 ) ) ;
#1521 = EDGE_CURVE ( 'NONE', #14564, #3602, #10864, .T. ) ;
#1522 = CARTESIAN_POINT ( 'NONE',  ( -7.690624001724057912, -48.30857337213000591, 17.76824091595882393 ) ) ;
#1523 = AXIS2_PLACEMENT_3D ( 'NONE', #11146, #10059, #8918 ) ;
#1524 = EDGE_CURVE ( 'NONE', #11896, #6476, #14383, .T. ) ;
#1525 = VECTOR ( 'NONE', #13691, 1000.000000000000000 ) ;
#1526 = AXIS2_PLACEMENT_3D ( 'NONE', #7238, #8475, #305 ) ;
#1527 = CARTESIAN_POINT ( 'NONE',  ( 15.96592141709277790, -29.94643662871589029, 3.810787175452606146 ) ) ;
#1528 = VERTEX_POINT ( 'NONE', #7408 ) ;
#1529 = CARTESIAN_POINT ( 'NONE',  ( -15.61203582817000068, -106.9748017008338365, -5.104852750214476487 ) ) ;
#1530 = DIRECTION ( 'NONE',  ( 0.000000000000000000, -1.000000000000000000, -1.224646799147350002E-16 ) ) ;
#1531 = CARTESIAN_POINT ( 'NONE',  ( 2.143005335038563608, 8.120575443056516463, 31.26488582106640024 ) ) ;
#1532 = ORIENTED_EDGE ( 'NONE', *, *, #14867, .T. ) ;
#1534 = EDGE_LOOP ( 'NONE', ( #4719, #13247, #10313, #11778 ) ) ;
#1533 = CARTESIAN_POINT ( 'NONE',  ( -17.81448839017816965, -11.78253482624722182, 56.75231026484397745 ) ) ;
#1535 = EDGE_CURVE ( 'NONE', #413, #14491, #6253, .T. ) ;
#1536 = VERTEX_POINT ( 'NONE', #6624 ) ;
#1537 = EDGE_CURVE ( 'NONE', #2093, #11647, #5320, .T. ) ;
#1538 = PLANE ( 'NONE',  #2993 ) ;
#1539 = VERTEX_POINT ( 'NONE', #13464 ) ;
#1540 = AXIS2_PLACEMENT_3D ( 'NONE', #1483, #9361, #14033 ) ;
#1541 = CARTESIAN_POINT ( 'NONE',  ( -11.16775676328319200, -22.49263881059494707, 56.85231026484400019 ) ) ;
#1542 = DIRECTION ( 'NONE',  ( -8.018662683283438208E-16, 5.975035461963189015E-16, 1.000000000000000000 ) ) ;
#1543 = SHAPE_DEFINITION_REPRESENTATION ( #9665, #2852 ) ;
#1544 = CARTESIAN_POINT ( 'NONE',  ( -5.898712304418589625, -10.80152183767200214, 56.85231026484400019 ) ) ;
#1545 = AXIS2_PLACEMENT_3D ( 'NONE', #4527, #15074, #2156 ) ;
#1546 = PLANE ( 'NONE',  #10322 ) ;
#1547 = DIRECTION ( 'NONE',  ( 0.000000000000000000, 0.5150380749100579303, 0.8571673007021101132 ) ) ;
#1548 = AXIS2_PLACEMENT_3D ( 'NONE', #12898, #7977, #5837 ) ;
#1549 = ORIENTED_EDGE ( 'NONE', *, *, #5722, .F. ) ;
#1550 = CARTESIAN_POINT ( 'NONE',  ( -11.55178736972959008, -19.37894070656199474, 57.00231026484399166 ) ) ;
#1551 = PRESENTATION_STYLE_ASSIGNMENT (( #7042 ) ) ;
#1552 = ORIENTED_EDGE ( 'NONE', *, *, #14224, .F. ) ;
#1553 = VERTEX_POINT ( 'NONE', #4428 ) ;
#1554 = EDGE_CURVE ( 'NONE', #12810, #14661, #10938, .T. ) ;
#1555 = CARTESIAN_POINT ( 'NONE',  ( -14.84437367148764686, -93.78075803281299727, -10.82899037021154953 ) ) ;
#1556 = EDGE_LOOP ( 'NONE', ( #448, #12545, #14683, #10579, #5127, #3544, #6237 ) ) ;
#1557 = ORIENTED_EDGE ( 'NONE', *, *, #2972, .T. ) ;
#1558 = FACE_OUTER_BOUND ( 'NONE', #9767, .T. ) ;
#1559 = DIRECTION ( 'NONE',  ( 0.000000000000000000, 0.000000000000000000, 1.000000000000000000 ) ) ;
#1560 = LINE ( 'NONE', #1630, #4366 ) ;
#1561 = VECTOR ( 'NONE', #8756, 1000.000000000000000 ) ;
#1562 = DIRECTION ( 'NONE',  ( -8.018662683283439195E-16, 5.975035461963190001E-16, 1.000000000000000000 ) ) ;
#1564 = CARTESIAN_POINT ( 'NONE',  ( -20.00744539586189319, -5.630737564061013778, 56.85231026484398598 ) ) ;
#1563 = DIRECTION ( 'NONE',  ( 0.5975035461963189576, 0.8018662683283437342, 0.000000000000000000 ) ) ;
#1565 = ORIENTED_EDGE ( 'NONE', *, *, #12915, .F. ) ;
#1566 = DIRECTION ( 'NONE',  ( 0.000000000000000000, 1.850371707708594316E-16, -1.000000000000000000 ) ) ;
#1567 = CARTESIAN_POINT ( 'NONE',  ( -31.79969986081099975, 11.99262100756199878, 24.16206422150099797 ) ) ;
#1568 = VERTEX_POINT ( 'NONE', #14826 ) ;
#1569 = VERTEX_POINT ( 'NONE', #6553 ) ;
#1570 = AXIS2_PLACEMENT_3D ( 'NONE', #2650, #9954, #708 ) ;
#1571 = EDGE_CURVE ( 'NONE', #13071, #7355, #12161, .T. ) ;
#1572 = CARTESIAN_POINT ( 'NONE',  ( -24.88854884048805971, -16.87637585156647191, 57.00231026484397745 ) ) ;
#1573 = ORIENTED_EDGE ( 'NONE', *, *, #10585, .T. ) ;
#1574 = EDGE_CURVE ( 'NONE', #2365, #4448, #9080, .T. ) ;
#1575 = CARTESIAN_POINT ( 'NONE',  ( 2.500300139188999626, -46.50737899243799944, 17.00231026484399877 ) ) ;
#1576 = DIRECTION ( 'NONE',  ( 0.000000000000000000, -1.000000000000000000, -1.224646799147350002E-16 ) ) ;
#1577 = CARTESIAN_POINT ( 'NONE',  ( -24.32830346761242879, -18.15026423267100597, 57.00231026484397745 ) ) ;
#1578 = CARTESIAN_POINT ( 'NONE',  ( -24.93814746875458610, -16.73481322911949931, 54.00231026484397745 ) ) ;
#1579 = VERTEX_POINT ( 'NONE', #3200 ) ;
#1580 = DIRECTION ( 'NONE',  ( -0.6780482080269577549, -0.7350174335289139105, -1.045284632676540317E-16 ) ) ;
#1581 = FACE_OUTER_BOUND ( 'NONE', #12812, .T. ) ;
#1582 = VERTEX_POINT ( 'NONE', #3280 ) ;
#1583 = EDGE_CURVE ( 'NONE', #10777, #12656, #11084, .T. ) ;
#1585 = EDGE_CURVE ( 'NONE', #2658, #9374, #4852, .T. ) ;
#1584 = CARTESIAN_POINT ( 'NONE',  ( -23.40321606353253614, -15.16438883951732741, 56.85231026484398598 ) ) ;
#1586 = DIRECTION ( 'NONE',  ( 0.5975035461963189576, 0.8018662683283437342, 0.000000000000000000 ) ) ;
#1587 = ORIENTED_EDGE ( 'NONE', *, *, #9618, .T. ) ;
#1588 = PLANE ( 'NONE',  #7166 ) ;
#1589 = ORIENTED_EDGE ( 'NONE', *, *, #6607, .T. ) ;
#1590 = VECTOR ( 'NONE', #4024, 1000.000000000000000 ) ;
#1591 = ADVANCED_FACE ( 'NONE', ( #4273 ), #3045, .T. ) ;
#1592 = CARTESIAN_POINT ( 'NONE',  ( -37.04494295528539993, 12.99262100756199878, 16.16206422150100153 ) ) ;
#1593 = ADVANCED_FACE ( 'NONE', ( #836 ), #7701, .T. ) ;
#1594 = CARTESIAN_POINT ( 'NONE',  ( -17.72867398697626129, -22.30470383268854562, 56.85231026484400019 ) ) ;
#1595 = DIRECTION ( 'NONE',  ( -0.9225966037272086417, 0.3857661296576204712, -9.702957262759976898E-16 ) ) ;
#1596 = PLANE ( 'NONE',  #9628 ) ;
#1597 = EDGE_LOOP ( 'NONE', ( #8667, #7626, #13250, #7951 ) ) ;
#1598 = CARTESIAN_POINT ( 'NONE',  ( 9.000300139189000959, -27.00737899243800300, 43.21206422150100224 ) ) ;
#1599 = CARTESIAN_POINT ( 'NONE',  ( -33.81844200665902633, -40.24211141608020625, 52.22352481299739679 ) ) ;
#1600 = ORIENTED_EDGE ( 'NONE', *, *, #3069, .F. ) ;
#1601 = CARTESIAN_POINT ( 'NONE',  ( -8.667632128016617088, -19.48099602858229318, 56.85231026484400019 ) ) ;
#1602 = EDGE_CURVE ( 'NONE', #5522, #11803, #496, .T. ) ;
#1603 = EDGE_CURVE ( 'NONE', #2842, #10291, #8931, .T. ) ;
#1604 = ORIENTED_EDGE ( 'NONE', *, *, #7269, .F. ) ;
#1606 = VERTEX_POINT ( 'NONE', #14906 ) ;
#1605 = CARTESIAN_POINT ( 'NONE',  ( -38.49969986081099904, -37.00737899243799944, -10.11609617439569675 ) ) ;
#1607 = VERTEX_POINT ( 'NONE', #7074 ) ;
#1608 = CARTESIAN_POINT ( 'NONE',  ( -15.49969986081092088, -13.50737899243822504, 57.00231026484397745 ) ) ;
#1609 = VERTEX_POINT ( 'NONE', #11610 ) ;
#1610 = DIRECTION ( 'NONE',  ( 0.000000000000000000, 0.1872998510044689147, 0.9823027872370635460 ) ) ;
#1611 = VECTOR ( 'NONE', #14316, 1000.000000000000114 ) ;
#1612 = DIRECTION ( 'NONE',  ( -8.018662683283438208E-16, 5.975035461963189015E-16, 1.000000000000000000 ) ) ;
#1613 = SHAPE_DEFINITION_REPRESENTATION ( #2577, #2372 ) ;
#1614 = PRODUCT_RELATED_PRODUCT_CATEGORY ( 'part', '', ( #264 ) ) ;
#1615 = B_SPLINE_CURVE_WITH_KNOTS ( 'NONE', 3,
 ( #1242, #6957, #4615, #9352, #3461, #8428, #8271, #2470, #3541, #7116, #2399, #14175, #12811, #11799, #5978, #7268, #182, #11957, #1395, #1166, #10650, #10502, #4694, #14023, #8196, #4846, #7040, #10577, #4769, #4921, #9427, #3693, #13040, #7196, #11874, #6047 ),
 .UNSPECIFIED., .F., .F.,
 ( 4, 2, 1, 1, 1, 2, 2, 2, 1, 1, 1, 2, 2, 2, 2, 2, 2, 2, 2, 2, 4 ),
 ( 0.000000000000000000, 0.1249999999999999722, 0.1875000000000001110, 0.2187500000000004996, 0.2343750000000006661, 0.2421875000000008049, 0.2500000000000009437, 0.3749999999999957256, 0.4374999999999933387, 0.4687499999999920064, 0.4843749999999903966, 0.4921874999999891198, 0.4999999999999878431, 0.6249999999999860112, 0.6874999999999842348, 0.7187499999999843459, 0.7499999999999844569, 0.8124999999999865663, 0.8437499999999887867, 0.8749999999999910072, 1.000000000000000000 ),
 .UNSPECIFIED. ) ;
#1616 = CYLINDRICAL_SURFACE ( 'NONE', #9730, 2.000000000000001776 ) ;
#1617 = EDGE_CURVE ( 'NONE', #7427, #6732, #1277, .T. ) ;
#1618 = DIRECTION ( 'NONE',  ( 1.011922027653136551E-15, -1.000000000000000000, 0.000000000000000000 ) ) ;
#1619 = CARTESIAN_POINT ( 'NONE',  ( -23.42445533997705454, -9.084766574938008432, 57.00231026484397745 ) ) ;
#1620 = CARTESIAN_POINT ( 'NONE',  ( -15.57469986081099478, -26.50737899243800300, 56.85231026484400019 ) ) ;
#1621 = EDGE_LOOP ( 'NONE', ( #3160, #7243 ) ) ;
#1622 = AXIS2_PLACEMENT_3D ( 'NONE', #12860, #14073, #5730 ) ;
#1623 = LINE ( 'NONE', #14403, #9014 ) ;
#1624 = ORIENTED_EDGE ( 'NONE', *, *, #3004, .T. ) ;
#1625 = VERTEX_POINT ( 'NONE', #9155 ) ;
#1626 = CARTESIAN_POINT ( 'NONE',  ( -15.49969986081099904, 12.99262100756199878, 24.21206422150099868 ) ) ;
#1627 = ORIENTED_EDGE ( 'NONE', *, *, #6991, .F. ) ;
#1628 = CARTESIAN_POINT ( 'NONE',  ( -15.13173615696983276, -107.1622034095870077, -6.087689735156000204 ) ) ;
#1629 = CARTESIAN_POINT ( 'NONE',  ( -15.61203582816999891, -106.6563755045979605, -6.855836844165478006 ) ) ;
#1630 = CARTESIAN_POINT ( 'NONE',  ( -9.291286065451624054, -6.887949398765353060, 57.00231026484397745 ) ) ;
#1631 = AXIS2_PLACEMENT_3D ( 'NONE', #14464, #1542, #13474 ) ;
#1632 = EDGE_CURVE ( 'NONE', #2532, #6446, #6775, .T. ) ;
#1633 = AXIS2_PLACEMENT_3D ( 'NONE', #6667, #12733, #10192 ) ;
#1634 = PRODUCT_DEFINITION_SHAPE ( 'NONE', 'NONE',  #15135 ) ;
#1635 = DIRECTION ( 'NONE',  ( 0.9320450512859435044, -0.1973458207444490908, -0.3038859151196102726 ) ) ;
#1636 = ORIENTED_EDGE ( 'NONE', *, *, #3326, .F. ) ;
#1637 = DIRECTION ( 'NONE',  ( 1.000000000000000000, 1.000000000000000078E-15, 1.000000000000000078E-15 ) ) ;
#1638 = CIRCLE ( 'NONE', #4825, 8.000000000000003553 ) ;
#1639 = ORIENTED_EDGE ( 'NONE', *, *, #12846, .F. ) ;
#1640 = LINE ( 'NONE', #10596, #10649 ) ;
#1641 = ORIENTED_EDGE ( 'NONE', *, *, #13372, .F. ) ;
#1642 = ORIENTED_EDGE ( 'NONE', *, *, #12311, .T. ) ;
#1643 = CARTESIAN_POINT ( 'NONE',  ( -21.51730450772242875, -49.78533579282670729, 56.51672281561283029 ) ) ;
#1644 = VERTEX_POINT ( 'NONE', #2361 ) ;
#1645 = AXIS2_PLACEMENT_3D ( 'NONE', #1886, #3101, #7761 ) ;
#1646 = CARTESIAN_POINT ( 'NONE',  ( -23.37741044072812713, -11.73331557219068877, 57.00231026484397745 ) ) ;
#1647 = CARTESIAN_POINT ( 'NONE',  ( 4.904519586037782375, 5.977956585851564419, 18.88724033448293227 ) ) ;
#1648 = FACE_OUTER_BOUND ( 'NONE', #535, .T. ) ;
#1649 =( BOUNDED_CURVE ( )  B_SPLINE_CURVE ( 3, ( #2084, #6806, #7878, #11263 ),
 .UNSPECIFIED., .F., .T. ) 
 B_SPLINE_CURVE_WITH_KNOTS ( ( 4, 4 ),
 ( 3.646861569849260576, 4.712388980384689674 ),
 .UNSPECIFIED. ) 
 CURVE ( )  GEOMETRIC_REPRESENTATION_ITEM ( )  RATIONAL_B_SPLINE_CURVE ( ( 1.000000000000000000, 0.9076044213655485304, 0.9076044213655485304, 1.000000000000000000 ) ) 
 REPRESENTATION_ITEM ( '' )  );
#1650 = EDGE_CURVE ( 'NONE', #374, #13801, #1205, .T. ) ;
#1651 = CARTESIAN_POINT ( 'NONE',  ( -11.44877351069547444, -22.65069971201824828, 56.78273114525553922 ) ) ;
#1652 = AXIS2_PLACEMENT_3D ( 'NONE', #2112, #14959, #10439 ) ;
#1653 = FACE_OUTER_BOUND ( 'NONE', #3673, .T. ) ;
#1654 = CARTESIAN_POINT ( 'NONE',  ( -13.74242962142780478, -4.603826257390357668, 56.85231026484398598 ) ) ;
#1655 = AXIS2_PLACEMENT_3D ( 'NONE', #14779, #707, #9031 ) ;
#1656 = ORIENTED_EDGE ( 'NONE', *, *, #8795, .F. ) ;
#1657 = CARTESIAN_POINT ( 'NONE',  ( -31.13003983167857314, -27.07585217469822680, -9.967496158821944618 ) ) ;
#1658 = DIRECTION ( 'NONE',  ( -1.000000000000000000, 1.291538348938060198E-32, -1.054621095516909827E-16 ) ) ;
#1659 = ORIENTED_EDGE ( 'NONE', *, *, #14390, .F. ) ;
#1660 = APPLICATION_CONTEXT ( 'automotive_design' ) ;
#1661 = CARTESIAN_POINT ( 'NONE',  ( 21.93915798269402728, -24.55717426787524715, 22.06612857817768969 ) ) ;
#1662 = ORIENTED_EDGE ( 'NONE', *, *, #14574, .F. ) ;
#1663 = FACE_OUTER_BOUND ( 'NONE', #12423, .T. ) ;
#1664 = VECTOR ( 'NONE', #5646, 1000.000000000000000 ) ;
#1665 = DIRECTION ( 'NONE',  ( -8.018662683283438208E-16, 5.975035461963189015E-16, 1.000000000000000000 ) ) ;
#1666 = EDGE_CURVE ( 'NONE', #8353, #2842, #10464, .T. ) ;
#1667 = CARTESIAN_POINT ( 'NONE',  ( -17.54662770128649285, -5.179934221328323929, 57.00231026484397745 ) ) ;
#1668 = AXIS2_PLACEMENT_3D ( 'NONE', #14800, #2333, #11359 ) ;
#1669 = DIRECTION ( 'NONE',  ( -1.000000000000000000, -3.632077277826439854E-16, 0.000000000000000000 ) ) ;
#1670 = CARTESIAN_POINT ( 'NONE',  ( -15.49969986081091733, -13.50737899243822682, 54.00231026484399166 ) ) ;
#1671 = EDGE_CURVE ( 'NONE', #3333, #15014, #7014, .T. ) ;
#1672 = ORIENTED_EDGE ( 'NONE', *, *, #93, .F. ) ;
#1673 = PLANE ( 'NONE',  #438 ) ;
#1674 = AXIS2_PLACEMENT_3D ( 'NONE', #4104, #3026, #11144 ) ;
#1675 = CARTESIAN_POINT ( 'NONE',  ( -15.49969986081092088, -13.50737899243822504, 57.00231026484397745 ) ) ;
#1676 = EDGE_LOOP ( 'NONE', ( #3977, #3251, #588, #13714 ) ) ;
#1677 = ORIENTED_EDGE ( 'NONE', *, *, #8951, .T. ) ;
#1679 = VERTEX_POINT ( 'NONE', #5715 ) ;
#1678 = CARTESIAN_POINT ( 'NONE',  ( -34.09967183693625969, -39.60750234067455722, -13.06022564672880470 ) ) ;
#1680 = ADVANCED_FACE ( 'NONE', ( #14059 ), #10534, .F. ) ;
#1681 = ORIENTED_EDGE ( 'NONE', *, *, #7069, .T. ) ;
#1682 = CARTESIAN_POINT ( 'NONE',  ( -14.61203582817000246, -105.9033823877427096, -6.327714494218207086 ) ) ;
#1683 = DIRECTION ( 'NONE',  ( -8.018662683283439195E-16, 5.975035461963190001E-16, 1.000000000000000000 ) ) ;
#1684 = AXIS2_PLACEMENT_3D ( 'NONE', #7110, #4763, #11638 ) ;
#1685 = DIRECTION ( 'NONE',  ( 0.000000000000000000, -0.1872998510044521503, -0.9823027872370667657 ) ) ;
#1686 = ADVANCED_FACE ( 'NONE', ( #10613 ), #12691, .T. ) ;
#1687 = DIRECTION ( 'NONE',  ( -0.9757243316563987134, -0.01146169732403567489, -0.2187022133132769386 ) ) ;
#1688 = EDGE_CURVE ( 'NONE', #2290, #10422, #8075, .T. ) ;
#1689 = DIRECTION ( 'NONE',  ( 1.000000000000000000, 1.000000000000000078E-15, 0.000000000000000000 ) ) ;
#1690 = DIRECTION ( 'NONE',  ( -8.018662683283439195E-16, 5.975035461963190001E-16, 1.000000000000000000 ) ) ;
#1691 = AXIS2_PLACEMENT_3D ( 'NONE', #13154, #147, #9464 ) ;
#1692 = TOROIDAL_SURFACE ( 'NONE', #10243, 28.00000000000000000, 5.000000000000000000 ) ;
#1693 = CARTESIAN_POINT ( 'NONE',  ( -7.514648799889656061, -44.01807676418170701, 44.76925787528261225 ) ) ;
#1694 = ORIENTED_EDGE ( 'NONE', *, *, #10377, .F. ) ;
#1695 = LINE ( 'NONE', #3991, #10549 ) ;
#1696 = ORIENTED_EDGE ( 'NONE', *, *, #1250, .T. ) ;
#1697 = LINE ( 'NONE', #12108, #10242 ) ;
#1699 = VERTEX_POINT ( 'NONE', #4805 ) ;
#1698 = CARTESIAN_POINT ( 'NONE',  ( -7.494881439401115841, -44.62162220065265217, -7.150567461381952761 ) ) ;
#1700 = ORIENTED_EDGE ( 'NONE', *, *, #1117, .T. ) ;
#1701 = CARTESIAN_POINT ( 'NONE',  ( -19.19431052208641475, -4.241825740657185762, 56.85231026484398598 ) ) ;
#1702 = EDGE_LOOP ( 'NONE', ( #14521, #4716, #7340, #8875, #13707, #9134, #14958, #5986, #6909, #10932 ) ) ;
#1703 = CYLINDRICAL_SURFACE ( 'NONE', #2024, 4.499999999999999112 ) ;
#1704 = AXIS2_PLACEMENT_3D ( 'NONE', #5318, #808, #4025 ) ;
#1705 = LINE ( 'NONE', #11193, #12472 ) ;
#1706 = CARTESIAN_POINT ( 'NONE',  ( -13.74242962142780478, -4.603826257390357668, 57.00231026484397745 ) ) ;
#1707 = ADVANCED_FACE ( 'NONE', ( #5858 ), #4654, .F. ) ;
#1708 = VECTOR ( 'NONE', #7051, 1000.000000000000000 ) ;
#1710 = CARTESIAN_POINT ( 'NONE',  ( -1.821162622431176770, -49.50737899243799944, -5.497689735156000346 ) ) ;
#1709 = CYLINDRICAL_SURFACE ( 'NONE', #9094, 0.4000000000000002998 ) ;
#1711 = ORIENTED_EDGE ( 'NONE', *, *, #7591, .T. ) ;
#1712 = CARTESIAN_POINT ( 'NONE',  ( 6.045543233663400073, 0.9926210075619987805, 32.26206422150099939 ) ) ;
#1713 = ORIENTED_EDGE ( 'NONE', *, *, #288, .T. ) ;
#1714 = DIRECTION ( 'NONE',  ( -1.000000000000000000, 0.000000000000000000, -1.011922027653137143E-15 ) ) ;
#1715 = ORIENTED_EDGE ( 'NONE', *, *, #9916, .F. ) ;
#1716 = ORIENTED_EDGE ( 'NONE', *, *, #3102, .T. ) ;
#1717 = DIRECTION ( 'NONE',  ( -1.000000000000000472E-15, 0.9823027872370664326, -0.1872998510044540932 ) ) ;
#1718 = ORIENTED_EDGE ( 'NONE', *, *, #227, .F. ) ;
#1720 = EDGE_CURVE ( 'NONE', #14153, #8778, #13833, .T. ) ;
#1719 = CARTESIAN_POINT ( 'NONE',  ( -15.83606446161809167, -16.37446674635458521, 51.00231026484399166 ) ) ;
#1721 = VECTOR ( 'NONE', #9876, 1000.000000000000000 ) ;
#1722 = DIRECTION ( 'NONE',  ( 0.09252159378507134047, -0.9957106782009873536, 6.691306063588577540E-16 ) ) ;
#1723 = DIRECTION ( 'NONE',  ( 0.000000000000000000, 1.000000000000000000, 1.224646799147350002E-16 ) ) ;
#1724 = CARTESIAN_POINT ( 'NONE',  ( 1.760741030006599317, 10.68321993080349763, 32.15417856559049881 ) ) ;
#1725 = CARTESIAN_POINT ( 'NONE',  ( -15.49969986081095996, -67.00737899243799234, -5.497689735156000346 ) ) ;
#1726 = FACE_OUTER_BOUND ( 'NONE', #5471, .T. ) ;
#1727 = ORIENTED_EDGE ( 'NONE', *, *, #13289, .F. ) ;
#1728 = DIRECTION ( 'NONE',  ( -1.000000000000000000, -1.000000000000000078E-15, -1.000000000000000078E-15 ) ) ;
#1729 = DIRECTION ( 'NONE',  ( -0.04695496274985035828, -0.9988970074402867549, 5.591929034707432303E-16 ) ) ;
#1730 = ORIENTED_EDGE ( 'NONE', *, *, #418, .F. ) ;
#1731 = CARTESIAN_POINT ( 'NONE',  ( 21.96532791796805739, -24.18694564958964222, 25.84096742429681726 ) ) ;
#1732 = CYLINDRICAL_SURFACE ( 'NONE', #8478, 22.99999999999999645 ) ;
#1733 = ORIENTED_EDGE ( 'NONE', *, *, #1808, .F. ) ;
#1734 = DIRECTION ( 'NONE',  ( 0.1165201156931293391, 0.9931883319083343320, -4.999999999999998416E-16 ) ) ;
#1735 = VERTEX_POINT ( 'NONE', #9231 ) ;
#1736 = DIRECTION ( 'NONE',  ( 0.5975035461963189576, 0.8018662683283437342, 0.000000000000000000 ) ) ;
#1737 = EDGE_CURVE ( 'NONE', #1827, #4959, #9779, .T. ) ;
#1738 = VECTOR ( 'NONE', #3700, 1000.000000000000227 ) ;
#1739 = LINE ( 'NONE', #11076, #9021 ) ;
#1740 = CARTESIAN_POINT ( 'NONE',  ( -7.567013331128944031, -48.78395362562287829, 18.42951909465858407 ) ) ;
#1741 = B_SPLINE_CURVE_WITH_KNOTS ( 'NONE', 3,
 ( #1015, #2238, #2320, #9117, #13795, #14020, #10499, #11419, #6886, #15010, #11570, #3313, #28, #7887, #10344, #9270, #15086, #10268, #14863, #4537, #9187, #2092, #8115, #14935, #4691, #13867 ),
 .UNSPECIFIED., .F., .F.,
 ( 4, 2, 2, 2, 2, 2, 2, 2, 2, 2, 2, 2, 4 ),
 ( 0.02522174898566975285, 0.02600993856294867707, 0.02679812814022759782, 0.02837450729478542544, 0.02916269687206434619, 0.02995088644934326694, 0.03152726560390109456, 0.03231545518118000143, 0.03310364475845890830, 0.03389183433573780824, 0.03468002391301671511, 0.03625640306757453579, 0.03783278222213234954 ),
 .UNSPECIFIED. ) ;
#1742 = DIRECTION ( 'NONE',  ( 8.018662683283438208E-16, -5.975035461963189015E-16, -1.000000000000000000 ) ) ;
#1743 = FACE_OUTER_BOUND ( 'NONE', #13369, .T. ) ;
#1744 = ORIENTED_EDGE ( 'NONE', *, *, #4194, .F. ) ;
#1745 = DIRECTION ( 'NONE',  ( 0.000000000000000000, 0.000000000000000000, 1.000000000000000000 ) ) ;
#1746 = DIRECTION ( 'NONE',  ( 0.9635179096299408830, -0.05012965580939084814, -0.2629073133839778253 ) ) ;
#1747 = VECTOR ( 'NONE', #6276, 1000.000000000000000 ) ;
#1748 = DIRECTION ( 'NONE',  ( 0.7071067811865487940, -0.1324409947604786031, -0.6945929620337749633 ) ) ;
#1749 = EDGE_LOOP ( 'NONE', ( #9395, #13866, #8340, #4658 ) ) ;
#1750 = VERTEX_POINT ( 'NONE', #10308 ) ;
#1752 = ORIENTED_EDGE ( 'NONE', *, *, #14125, .F. ) ;
#1751 = CARTESIAN_POINT ( 'NONE',  ( 2.500300139188999182, -46.50737899243799944, -5.497689735156002122 ) ) ;
#1753 = VERTEX_POINT ( 'NONE', #11682 ) ;
#1754 = EDGE_CURVE ( 'NONE', #8324, #7478, #4887, .T. ) ;
#1755 = CARTESIAN_POINT ( 'NONE',  ( -15.49969986081099904, -13.50737899243800122, 6.712064221500998684 ) ) ;
#1756 = LINE ( 'NONE', #13252, #4629 ) ;
#1757 = ADVANCED_FACE ( 'NONE', ( #8542 ), #14434, .T. ) ;
#1758 = AXIS2_PLACEMENT_3D ( 'NONE', #6517, #13287, #12127 ) ;
#1759 = DIRECTION ( 'NONE',  ( -8.018662683283438208E-16, 5.975035461963189015E-16, 1.000000000000000000 ) ) ;
#1760 = CARTESIAN_POINT ( 'NONE',  ( -32.89073566799068971, 9.431003388506304930, 16.55506475363483787 ) ) ;
#1761 = VECTOR ( 'NONE', #9432, 1000.000000000000000 ) ;
#1762 = AXIS2_PLACEMENT_3D ( 'NONE', #4116, #9853, #7473 ) ;
#1763 = FACE_OUTER_BOUND ( 'NONE', #4849, .T. ) ;
#1764 = DIRECTION ( 'NONE',  ( 0.5975035461963217331, 0.8018662683283416248, 0.000000000000000000 ) ) ;
#1765 = DIRECTION ( 'NONE',  ( 0.000000000000000000, -1.000000000000000000, -1.224646799147350002E-16 ) ) ;
#1766 = ADVANCED_FACE ( 'NONE', ( #7389 ), #6085, .T. ) ;
#1767 = LINE ( 'NONE', #1619, #12286 ) ;
#1768 = ORIENTED_EDGE ( 'NONE', *, *, #8455, .T. ) ;
#1769 = CARTESIAN_POINT ( 'NONE',  ( -15.49969986081086226, -13.50737899243826767, -13.49768973515600301 ) ) ;
#1770 = AXIS2_PLACEMENT_3D ( 'NONE', #8491, #537, #4989 ) ;
#1771 = ORIENTED_EDGE ( 'NONE', *, *, #1860, .F. ) ;
#1772 = LINE ( 'NONE', #12034, #5116 ) ;
#1774 = ORIENTED_EDGE ( 'NONE', *, *, #7676, .T. ) ;
#1773 = DIRECTION ( 'NONE',  ( -8.018662683283438208E-16, 5.975035461963189015E-16, 1.000000000000000000 ) ) ;
#1775 = ORIENTED_EDGE ( 'NONE', *, *, #8960, .T. ) ;
#1776 = AXIS2_PLACEMENT_3D ( 'NONE', #10188, #5823, #5598 ) ;
#1777 = EDGE_CURVE ( 'NONE', #5054, #364, #6270, .T. ) ;
#1778 = DIRECTION ( 'NONE',  ( 0.1511109077013141899, 0.9885168150181791180, -4.694715627858909121E-16 ) ) ;
#1779 = ADVANCED_FACE ( 'NONE', ( #1581 ), #12073, .F. ) ;
#1781 = VERTEX_POINT ( 'NONE', #2584 ) ;
#1780 = CARTESIAN_POINT ( 'NONE',  ( -15.49969986081099549, 0.9926210075620015560, 1.212064221501000461 ) ) ;
#1782 = B_SPLINE_CURVE_WITH_KNOTS ( 'NONE', 3,
 ( #820, #4181, #12015, #1531, #8834, #8916, #12369, #13596, #6184, #2755, #10057, #5476 ),
 .UNSPECIFIED., .F., .F.,
 ( 4, 2, 2, 2, 2, 4 ),
 ( 0.000000000000000000, 0.2500000000000004441, 0.3750000000000000000, 0.4374999999999991673, 0.4999999999999983347, 1.000000000000000000 ),
 .UNSPECIFIED. ) ;
#1783 = DIRECTION ( 'NONE',  ( -8.018662683283438208E-16, 5.975035461963189015E-16, 1.000000000000000000 ) ) ;
#1784 = ADVANCED_FACE ( 'NONE', ( #11995 ), #3879, .F. ) ;
#1785 = DIRECTION ( 'NONE',  ( -0.4177292884839868270, -0.9085715390340278752, 2.079116908177700458E-16 ) ) ;
#1786 = DIRECTION ( 'NONE',  ( -8.018662683283438208E-16, 5.975035461963189015E-16, 1.000000000000000000 ) ) ;
#1787 = EDGE_CURVE ( 'NONE', #12721, #8099, #189, .T. ) ;
#1788 = AXIS2_PLACEMENT_3D ( 'NONE', #11706, #10637, #11860 ) ;
#1790 = CARTESIAN_POINT ( 'NONE',  ( -22.61924992783766797, -9.696439889920343447, 56.85231026484398598 ) ) ;
#1789 = CARTESIAN_POINT ( 'NONE',  ( -24.36945568363038461, -11.58678490633884373, 56.85231026484398598 ) ) ;
#1791 = ORIENTED_EDGE ( 'NONE', *, *, #14783, .F. ) ;
#1792 = CARTESIAN_POINT ( 'NONE',  ( -18.10194853779420043, -23.13696500758647190, 54.00231026484399166 ) ) ;
#1793 = VERTEX_POINT ( 'NONE', #6232 ) ;
#1794 = LINE ( 'NONE', #13351, #11380 ) ;
#1795 = ORIENTED_EDGE ( 'NONE', *, *, #4686, .F. ) ;
#1796 = ORIENTED_EDGE ( 'NONE', *, *, #5413, .F. ) ;
#1797 = CARTESIAN_POINT ( 'NONE',  ( -19.05417371652952951, -51.69327491641966787, 56.83659220636065612 ) ) ;
#1798 = EDGE_CURVE ( 'NONE', #12241, #7870, #8495, .T. ) ;
#1799 = EDGE_CURVE ( 'NONE', #8578, #14370, #1638, .T. ) ;
#1800 = ORIENTED_EDGE ( 'NONE', *, *, #12612, .T. ) ;
#1801 = CARTESIAN_POINT ( 'NONE',  ( -7.886584594865190034, -46.96511696614950182, -7.955427708867500058 ) ) ;
#1802 = VECTOR ( 'NONE', #6555, 1000.000000000000114 ) ;
#1803 = EDGE_CURVE ( 'NONE', #1165, #7506, #4327, .T. ) ;
#1804 = AXIS2_PLACEMENT_3D ( 'NONE', #11529, #1055, #10988 ) ;
#1805 = LINE ( 'NONE', #6304, #10117 ) ;
#1806 = PLANE ( 'NONE',  #1704 ) ;
#1807 = CARTESIAN_POINT ( 'NONE',  ( -12.11547932532413263, -20.83938426843124603, 57.00231026484399166 ) ) ;
#1808 = EDGE_CURVE ( 'NONE', #10889, #6707, #6009, .T. ) ;
#1809 = VECTOR ( 'NONE', #14780, 1000.000000000000000 ) ;
#1810 = CARTESIAN_POINT ( 'NONE',  ( -6.488891646287396675, -12.42729319905174634, 56.85231026484400019 ) ) ;
#1811 = DIRECTION ( 'NONE',  ( 0.5975035461963189576, 0.8018662683283437342, 0.000000000000000000 ) ) ;
#1812 = ORIENTED_EDGE ( 'NONE', *, *, #12702, .T. ) ;
#1813 = CARTESIAN_POINT ( 'NONE',  ( -33.37651573321840459, -23.18484177525213141, -8.848022433876742809 ) ) ;
#1814 = DIRECTION ( 'NONE',  ( -9.912705577010322591E-16, 0.1872998510044552312, 0.9823027872370662106 ) ) ;
#1815 = VERTEX_POINT ( 'NONE', #9845 ) ;
#1816 = CARTESIAN_POINT ( 'NONE',  ( 21.86105339610482545, -26.58130273022555912, 27.44097045403598401 ) ) ;
#1817 = DIRECTION ( 'NONE',  ( 3.632077277826439854E-16, -1.000000000000000000, 0.000000000000000000 ) ) ;
#1818 = CIRCLE ( 'NONE', #2057, 0.9999999999999990008 ) ;
#1819 = ORIENTED_EDGE ( 'NONE', *, *, #7358, .F. ) ;
#1820 = DIRECTION ( 'NONE',  ( 0.5975035461963189576, 0.8018662683283437342, 0.000000000000000000 ) ) ;
#1821 = AXIS2_PLACEMENT_3D ( 'NONE', #2282, #9459, #3277 ) ;
#1822 = DIRECTION ( 'NONE',  ( 0.8660254037844387076, 0.4999999999999998890, 0.000000000000000000 ) ) ;
#1823 = LINE ( 'NONE', #6469, #1887 ) ;
#1824 = EDGE_CURVE ( 'NONE', #2908, #4255, #3953, .T. ) ;
#1825 = PLANE ( 'NONE',  #5279 ) ;
#1826 = LINE ( 'NONE', #8927, #4996 ) ;
#1827 = VERTEX_POINT ( 'NONE', #513 ) ;
#1828 = CARTESIAN_POINT ( 'NONE',  ( -32.94709454773337143, 9.133458655302877816, 31.73466097731338209 ) ) ;
#1829 = DIRECTION ( 'NONE',  ( 8.018662683283438208E-16, -5.975035461963189015E-16, -1.000000000000000000 ) ) ;
#1830 = ORIENTED_EDGE ( 'NONE', *, *, #7449, .F. ) ;
#1832 = ORIENTED_EDGE ( 'NONE', *, *, #8780, .F. ) ;
#1831 = CARTESIAN_POINT ( 'NONE',  ( -35.65036695804911915, -37.88568168826260063, -12.12527094935855843 ) ) ;
#1833 = EDGE_LOOP ( 'NONE', ( #1115, #6516, #7526, #11408 ) ) ;
#1834 = DIRECTION ( 'NONE',  ( -0.5779813897169993053, 0.8160499452489450301, -9.510565162951571123E-16 ) ) ;
#1835 = CARTESIAN_POINT ( 'NONE',  ( -11.55238169831532957, -21.67927775123549594, 57.00231026484399166 ) ) ;
#1836 = B_SPLINE_CURVE_WITH_KNOTS ( 'NONE', 3,
 ( #9857, #459, #2890, #2744, #13164, #7324, #386, #12007, #9922, #3967, #8630, #14378, #5117, #8551, #14524, #1522, #7475, #12150, #2964, #8699, #7622, #13384, #1740, #10859, #5044, #3894, #13238, #7402, #6395, #12083, #11078, #14671, #6768, #7996, #2049, #10068, #3116, #978, #10226, #13679, #14820, #3040, #5633, #4191, #14750, #11233, #3195, #7839, #12531 ),
 .UNSPECIFIED., .F., .F.,
 ( 4, 2, 2, 1, 1, 2, 2, 2, 2, 1, 1, 2, 2, 2, 2, 2, 1, 2, 2, 2, 2, 2, 1, 1, 2, 2, 2, 4 ),
 ( 0.000000000000000000, 0.06249999999999369948, 0.09374999999998918920, 0.1093749999999871908, 0.1171874999999874128, 0.1210937499999866634, 0.1249999999999859279, 0.1874999999999953648, 0.2187500000000005274, 0.2343750000000031086, 0.2421875000000043299, 0.2460937500000049682, 0.2500000000000056066, 0.3750000000000073830, 0.4375000000000082712, 0.4687500000000087708, 0.4843750000000079936, 0.4921875000000084377, 0.5000000000000088818, 0.6250000000000403011, 0.6875000000000554001, 0.7187500000000633937, 0.7343750000000669464, 0.7421875000000682787, 0.7460937500000681677, 0.7500000000000679456, 0.8750000000000339728, 1.000000000000000000 ),
 .UNSPECIFIED. ) ;
#1837 = DIRECTION ( 'NONE',  ( 8.018662683283438208E-16, -5.975035461963189015E-16, -1.000000000000000000 ) ) ;
#1838 = CARTESIAN_POINT ( 'NONE',  ( -8.308948803761788682, -48.01658430907413333, 42.50291890924265914 ) ) ;
#1839 = AXIS2_PLACEMENT_3D ( 'NONE', #12023, #7569, #10876 ) ;
#1840 = CARTESIAN_POINT ( 'NONE',  ( -5.499699860810997265, -46.50737899243799944, -2.997689735156003010 ) ) ;
#1841 = CARTESIAN_POINT ( 'NONE',  ( -16.99345872630171428, -15.51204466325908982, 51.25231026484399166 ) ) ;
#1842 = EDGE_CURVE ( 'NONE', #7908, #8391, #3593, .T. ) ;
#1843 = DIRECTION ( 'NONE',  ( 1.000000000000000000, -1.291538348938060198E-32, 1.054621095516909827E-16 ) ) ;
#1844 = DIRECTION ( 'NONE',  ( -0.6061090314442014737, 0.7953815700667020705, -9.612616959383187437E-16 ) ) ;
#1845 = PLANE ( 'NONE',  #8363 ) ;
#1846 = ADVANCED_FACE ( 'NONE', ( #9616 ), #1510, .F. ) ;
#1847 = EDGE_LOOP ( 'NONE', ( #5397, #11160, #13721, #7720 ) ) ;
#1848 = CARTESIAN_POINT ( 'NONE',  ( 4.000300139189000959, -19.50737899243798879, -12.52892449124999885 ) ) ;
#1849 = ORIENTED_EDGE ( 'NONE', *, *, #1085, .T. ) ;
#1850 = PLANE ( 'NONE',  #6796 ) ;
#1851 = ORIENTED_EDGE ( 'NONE', *, *, #11118, .T. ) ;
#1852 = ORIENTED_EDGE ( 'NONE', *, *, #1484, .T. ) ;
#1853 = CARTESIAN_POINT ( 'NONE',  ( -9.328067836852527606, -18.71527762440592468, 56.85231026484400019 ) ) ;
#1855 = VERTEX_POINT ( 'NONE', #13073 ) ;
#1854 = CARTESIAN_POINT ( 'NONE',  ( 1.760741030006599317, 10.68321993080349763, 16.26994987741148790 ) ) ;
#1856 = VECTOR ( 'NONE', #7773, 1000.000000000000000 ) ;
#1857 = CARTESIAN_POINT ( 'NONE',  ( -10.99969986081099904, -13.50737899243800122, -13.01695671647155983 ) ) ;
#1858 = DIRECTION ( 'NONE',  ( 0.000000000000000000, 1.000000000000000000, 1.224646799147350002E-16 ) ) ;
#1859 = CARTESIAN_POINT ( 'NONE',  ( -6.540243082598547808, -14.95284924095401458, 56.85231026484400019 ) ) ;
#1860 = EDGE_CURVE ( 'NONE', #6476, #14925, #2660, .T. ) ;
#1861 = ADVANCED_FACE ( 'NONE', ( #1437 ), #4958, .F. ) ;
#1862 = CARTESIAN_POINT ( 'NONE',  ( -7.681929635180895666, -48.34577715838007350, -7.192553627470831046 ) ) ;
#1863 = AXIS2_PLACEMENT_3D ( 'NONE', #13846, #15066, #9479 ) ;
#1864 = DIRECTION ( 'NONE',  ( 8.018662683283438208E-16, -5.975035461963189015E-16, -1.000000000000000000 ) ) ;
#1865 = EDGE_CURVE ( 'NONE', #13612, #8489, #12217, .T. ) ;
#1866 = VERTEX_POINT ( 'NONE', #10213 ) ;
#1867 = CARTESIAN_POINT ( 'NONE',  ( -15.49969986081091555, -110.0073789924380065, -5.497689735155995017 ) ) ;
#1868 = CARTESIAN_POINT ( 'NONE',  ( -15.49969986081095996, -67.00737899243799234, -5.497689735156000346 ) ) ;
#1869 = EDGE_LOOP ( 'NONE', ( #3180, #14178, #2700, #3321 ) ) ;
#1870 = VERTEX_POINT ( 'NONE', #8913 ) ;
#1871 = DIRECTION ( 'NONE',  ( 0.000000000000000000, 1.000000000000000000, 1.224646799147350002E-16 ) ) ;
#1872 = ORIENTED_EDGE ( 'NONE', *, *, #12630, .F. ) ;
#1873 = ADVANCED_FACE ( 'NONE', ( #13516 ), #7826, .T. ) ;
#1874 = CARTESIAN_POINT ( 'NONE',  ( -15.49969986081099904, -44.50737899243799944, -109.5506571639849938 ) ) ;
#1875 = VECTOR ( 'NONE', #6712, 1000.000000000000000 ) ;
#1876 =( BOUNDED_CURVE ( )  B_SPLINE_CURVE ( 3, ( #237, #3751, #8408, #5957 ),
 .UNSPECIFIED., .F., .T. ) 
 B_SPLINE_CURVE_WITH_KNOTS ( ( 4, 4 ),
 ( 0.000000000000000000, 1.570796326794893893 ),
 .UNSPECIFIED. ) 
 CURVE ( )  GEOMETRIC_REPRESENTATION_ITEM ( )  RATIONAL_B_SPLINE_CURVE ( ( 1.000000000000000000, 0.8047378541243654926, 0.8047378541243654926, 1.000000000000000000 ) ) 
 REPRESENTATION_ITEM ( '' )  );
#1877 = DIRECTION ( 'NONE',  ( 0.1272150336605032961, -0.9918751611018177261, 6.946583704589934213E-16 ) ) ;
#1878 = CARTESIAN_POINT ( 'NONE',  ( -12.84854673063650132, -12.36513540471286454, 56.75231026484397745 ) ) ;
#1879 = CIRCLE ( 'NONE', #14342, 9.974999999999999645 ) ;
#1880 = EDGE_CURVE ( 'NONE', #2588, #6205, #14660, .T. ) ;
#1881 = LINE ( 'NONE', #2318, #8501 ) ;
#1882 = EDGE_CURVE ( 'NONE', #1083, #13264, #3103, .T. ) ;
#1883 = CARTESIAN_POINT ( 'NONE',  ( -31.79969986081099975, 11.99262100756199878, 16.16206422150100153 ) ) ;
#1884 = DIRECTION ( 'NONE',  ( 1.000000000000000000, -1.291538348938060198E-32, 1.054621095516909827E-16 ) ) ;
#1885 = ORIENTED_EDGE ( 'NONE', *, *, #12156, .T. ) ;
#1886 = CARTESIAN_POINT ( 'NONE',  ( -15.49969986081099904, 1010.738102757665843, 24.21206422150112303 ) ) ;
#1887 = VECTOR ( 'NONE', #3818, 1000.000000000000114 ) ;
#1888 = CARTESIAN_POINT ( 'NONE',  ( -15.49969986081099904, -13.50737899243800122, 6.712064221500998684 ) ) ;
#1889 = ORIENTED_EDGE ( 'NONE', *, *, #6659, .F. ) ;
#1890 = DIRECTION ( 'NONE',  ( -1.000000000000000000, 1.499759782661860071E-32, -1.224646799147350002E-16 ) ) ;
#1891 = CARTESIAN_POINT ( 'NONE',  ( 21.92052636685137657, -24.86057730259263820, 21.76261826740604377 ) ) ;
#1892 = CARTESIAN_POINT ( 'NONE',  ( -15.49969986081099904, -52.50737899243799944, 57.00231026484399166 ) ) ;
#1893 = EDGE_LOOP ( 'NONE', ( #5402, #520, #6069, #2568 ) ) ;
#1894 = CARTESIAN_POINT ( 'NONE',  ( -9.031792552787402784, -10.63903015472409486, 56.85231026484400019 ) ) ;
#1895 = CARTESIAN_POINT ( 'NONE',  ( -15.49969986081092088, -13.50737899243822504, 57.00231026484397745 ) ) ;
#1896 = VECTOR ( 'NONE', #5253, 1000.000000000000000 ) ;
#1897 = DIRECTION ( 'NONE',  ( 1.000000000000000000, 8.799128391690932181E-16, -4.979791928221684326E-16 ) ) ;
#1898 = PLANE ( 'NONE',  #1392 ) ;
#1899 = VECTOR ( 'NONE', #11749, 1000.000000000000000 ) ;
#1900 = CARTESIAN_POINT ( 'NONE',  ( -15.49969986081099904, -27.00737899243800300, -13.49768973515600301 ) ) ;
#1901 = CARTESIAN_POINT ( 'NONE',  ( -24.39712111458419130, -18.01698208283363556, 56.85231026484398598 ) ) ;
#1902 = EDGE_LOOP ( 'NONE', ( #9229, #10233 ) ) ;
#1903 = CARTESIAN_POINT ( 'NONE',  ( -3.508527451664999575, -46.50737899243799234, -5.497689735156000346 ) ) ;
#1904 = CARTESIAN_POINT ( 'NONE',  ( -7.730254068284388325, -46.40242140125007353, -2.999336575030471685 ) ) ;
#1905 = ORIENTED_EDGE ( 'NONE', *, *, #8887, .T. ) ;
#1906 = VECTOR ( 'NONE', #3559, 1000.000000000000000 ) ;
#1908 = VERTEX_POINT ( 'NONE', #10055 ) ;
#1907 = CARTESIAN_POINT ( 'NONE',  ( -8.525484111995742964, -7.700351810740323266, 57.00231026484399166 ) ) ;
#1909 = VERTEX_POINT ( 'NONE', #9984 ) ;
#1910 = FACE_OUTER_BOUND ( 'NONE', #5741, .T. ) ;
#1911 = VECTOR ( 'NONE', #8056, 1000.000000000000000 ) ;
#1912 = VECTOR ( 'NONE', #6196, 1000.000000000000114 ) ;
#1913 = FACE_OUTER_BOUND ( 'NONE', #2325, .T. ) ;
#1914 = PLANE ( 'NONE',  #9485 ) ;
#1915 = ADVANCED_FACE ( 'NONE', ( #5545 ), #9914, .T. ) ;
#1916 = ADVANCED_FACE ( 'NONE', ( #5473 ), #14736, .F. ) ;
#1917 = CARTESIAN_POINT ( 'NONE',  ( -20.39403028972282428, -7.084672814149619136, 56.85231026484398598 ) ) ;
#1918 = CARTESIAN_POINT ( 'NONE',  ( -8.371409249847948431, -48.14116718798079120, 46.40142299527308012 ) ) ;
#1919 = CARTESIAN_POINT ( 'NONE',  ( 22.00030013918900096, -27.00737899243800300, 21.71206422150100224 ) ) ;
#1920 = CARTESIAN_POINT ( 'NONE',  ( -15.83606446161808456, -16.37446674635458876, 51.10586365543726117 ) ) ;
#1921 = CARTESIAN_POINT ( 'NONE',  ( -15.49969986081099904, -13.50737899243800122, 51.00231026484400587 ) ) ;
#1922 = FACE_OUTER_BOUND ( 'NONE', #12201, .T. ) ;
#1923 = ORIENTED_EDGE ( 'NONE', *, *, #3003, .T. ) ;
#1924 = CARTESIAN_POINT ( 'NONE',  ( 14.82734454558327464, -28.13112904194727193, 46.26954949554266250 ) ) ;
#1925 = ORIENTED_EDGE ( 'NONE', *, *, #4586, .F. ) ;
#1926 = ORIENTED_EDGE ( 'NONE', *, *, #10584, .T. ) ;
#1927 = DIRECTION ( 'NONE',  ( 0.7276687409742212953, 0.6859287159822015090, 1.736481776669299976E-16 ) ) ;
#1928 = FACE_OUTER_BOUND ( 'NONE', #9172, .T. ) ;
#1930 = ORIENTED_EDGE ( 'NONE', *, *, #10174, .F. ) ;
#1929 = DIRECTION ( 'NONE',  ( 0.000000000000000000, 0.1872998510044759646, 0.9823027872370621028 ) ) ;
#1931 = CARTESIAN_POINT ( 'NONE',  ( -9.959408463899000807, -21.80230492564002276, 54.00231026484400587 ) ) ;
#1932 = ADVANCED_FACE ( 'NONE', ( #13668 ), #11289, .F. ) ;
#1933 = DIRECTION ( 'NONE',  ( -8.018662683283438208E-16, 5.975035461963189015E-16, 1.000000000000000000 ) ) ;
#1934 = VECTOR ( 'NONE', #10797, 1000.000000000000000 ) ;
#1935 = VECTOR ( 'NONE', #96, 1000.000000000000000 ) ;
#1936 = DIRECTION ( 'NONE',  ( -1.734723475976808080E-16, 0.000000000000000000, 1.000000000000000000 ) ) ;
#1937 = CARTESIAN_POINT ( 'NONE',  ( -16.02866194833901403, -110.0647956111179866, -10.55728977053499129 ) ) ;
#1938 = VECTOR ( 'NONE', #7417, 1000.000000000000114 ) ;
#1939 = ORIENTED_EDGE ( 'NONE', *, *, #13456, .F. ) ;
#1940 = CARTESIAN_POINT ( 'NONE',  ( 18.17382430658342685, -24.91495491142563878, 40.71553431842708903 ) ) ;
#1941 = ORIENTED_EDGE ( 'NONE', *, *, #7322, .T. ) ;
#1942 = CARTESIAN_POINT ( 'NONE',  ( -15.49969986081099904, 10.68321993080349763, 24.21206422150099868 ) ) ;
#1943 = ORIENTED_EDGE ( 'NONE', *, *, #4054, .T. ) ;
#1944 = VERTEX_POINT ( 'NONE', #4257 ) ;
#1945 = CARTESIAN_POINT ( 'NONE',  ( 21.88637859935752772, -28.44597745863666916, 21.29012428004587676 ) ) ;
#1946 = CARTESIAN_POINT ( 'NONE',  ( -8.971570239337626873, -21.04953708182106098, 57.00231026484399166 ) ) ;
#1947 = ORIENTED_EDGE ( 'NONE', *, *, #3648, .T. ) ;
#1948 = VECTOR ( 'NONE', #11790, 1000.000000000000000 ) ;
#1949 = AXIS2_PLACEMENT_3D ( 'NONE', #11524, #5708, #10378 ) ;
#1950 = CARTESIAN_POINT ( 'NONE',  ( -12.76843194806299842, -13.82780931059433271, 56.75231026484399166 ) ) ;
#1951 = EDGE_CURVE ( 'NONE', #12278, #8801, #816, .T. ) ;
#1952 = EDGE_CURVE ( 'NONE', #8358, #6010, #11068, .T. ) ;
#1954 = CARTESIAN_POINT ( 'NONE',  ( -5.526612771747946518, -13.70272205979775748, 56.85231026484400019 ) ) ;
#1953 =( REPRESENTATION_RELATIONSHIP ('NONE','NONE', #2372, #3931 ) REPRESENTATION_RELATIONSHIP_WITH_TRANSFORMATION ( #1051 )SHAPE_REPRESENTATION_RELATIONSHIP( ) );
#1955 = DIRECTION ( 'NONE',  ( 0.000000000000000000, -2.220446049250313081E-16, 1.000000000000000000 ) ) ;
#1956 = CARTESIAN_POINT ( 'NONE',  ( 4.185908152463202470, 11.99262100756819827, 16.16206422150100153 ) ) ;
#1957 = PLANE ( 'NONE',  #6193 ) ;
#1959 = CARTESIAN_POINT ( 'NONE',  ( -3.508527451665000463, -45.64135358865355840, -3.997689735156000790 ) ) ;
#1958 = DIRECTION ( 'NONE',  ( -1.734723475976805615E-16, 0.000000000000000000, 1.000000000000000000 ) ) ;
#1960 = VERTEX_POINT ( 'NONE', #10132 ) ;
#1961 = FACE_OUTER_BOUND ( 'NONE', #14494, .T. ) ;
#1962 = DIRECTION ( 'NONE',  ( 0.9040177279761104634, 0.4274949678123838859, 4.694715627858909121E-16 ) ) ;
#1963 = ADVANCED_FACE ( 'NONE', ( #14808 ), #7762, .T. ) ;
#1964 = ORIENTED_EDGE ( 'NONE', *, *, #10838, .T. ) ;
#1965 = FACE_OUTER_BOUND ( 'NONE', #9078, .T. ) ;
#1966 = TOROIDAL_SURFACE ( 'NONE', #5375, 1.600000000000000089, 0.1499999999999999944 ) ;
#1967 = CARTESIAN_POINT ( 'NONE',  ( -18.43409448121630945, -5.984417261063049942, 56.85231026484398598 ) ) ;
#1968 = LINE ( 'NONE', #10061, #12820 ) ;
#1969 = ORIENTED_EDGE ( 'NONE', *, *, #4536, .T. ) ;
#1970 = DIRECTION ( 'NONE',  ( 0.000000000000000000, 0.000000000000000000, -1.000000000000000000 ) ) ;
#1971 = EDGE_CURVE ( 'NONE', #14676, #7782, #5575, .T. ) ;
#1972 = ADVANCED_FACE ( 'NONE', ( #11220 ), #737, .F. ) ;
#1973 = ADVANCED_FACE ( 'NONE', ( #12514 ), #2035, .T. ) ;
#1974 = CARTESIAN_POINT ( 'NONE',  ( -15.45180655762527699, -13.52173975529984418, 56.85231026484398598 ) ) ;
#1975 = APPLICATION_PROTOCOL_DEFINITION ( 'draft international standard', 'automotive_design', 1998, #13971 ) ;
#1976 = CARTESIAN_POINT ( 'NONE',  ( -15.49969986081099904, 2.992621007561997004, 24.21206422150099868 ) ) ;
#1977 = DIRECTION ( 'NONE',  ( -1.000000000000000000, 0.000000000000000000, 0.000000000000000000 ) ) ;
#1978 = ORIENTED_EDGE ( 'NONE', *, *, #14200, .T. ) ;
#1979 = CARTESIAN_POINT ( 'NONE',  ( -15.49969986081099016, -110.4502521595424298, -11.13806342361127832 ) ) ;
#1980 = CARTESIAN_POINT ( 'NONE',  ( -18.15085299098534577, -14.64962258016358199, 56.75231026484397745 ) ) ;
#1981 = VERTEX_POINT ( 'NONE', #4033 ) ;
#1983 = ORIENTED_EDGE ( 'NONE', *, *, #3367, .F. ) ;
#1982 = DIRECTION ( 'NONE',  ( -1.000000000000000000, -3.839882694219489529E-17, 0.000000000000000000 ) ) ;
#1984 = EDGE_LOOP ( 'NONE', ( #3084, #3204, #2775, #5347 ) ) ;
#1985 = LINE ( 'NONE', #7783, #11547 ) ;
#1986 = DIRECTION ( 'NONE',  ( -9.912705577010322591E-16, 0.1872998510044552312, 0.9823027872370662106 ) ) ;
#1987 = EDGE_CURVE ( 'NONE', #5856, #642, #8685, .T. ) ;
#1988 = DIRECTION ( 'NONE',  ( -0.9957106782009873536, -0.09252159378507134047, -7.431448254773946593E-16 ) ) ;
#1989 = CARTESIAN_POINT ( 'NONE',  ( -15.49969986081099904, -27.00737899243799944, -5.497689735156000346 ) ) ;
#1990 = CARTESIAN_POINT ( 'NONE',  ( -5.499699860811003482, -46.50737899243799944, 44.50231026484399877 ) ) ;
#1991 = CIRCLE ( 'NONE', #10540, 8.886381701226328644 ) ;
#1992 = CARTESIAN_POINT ( 'NONE',  ( 22.00030013918900096, -27.00737899243800300, 5.212064221501000461 ) ) ;
#1993 = DIRECTION ( 'NONE',  ( -8.018662683283438208E-16, 5.975035461963189015E-16, 1.000000000000000000 ) ) ;
#1994 = EDGE_CURVE ( 'NONE', #7908, #1793, #3332, .T. ) ;
#1995 = LINE ( 'NONE', #9171, #10574 ) ;
#1996 = CARTESIAN_POINT ( 'NONE',  ( 18.30004068436167231, -28.74307097840769742, 40.45547825031584921 ) ) ;
#1997 = ORIENTED_EDGE ( 'NONE', *, *, #12650, .T. ) ;
#1998 = LINE ( 'NONE', #10691, #3351 ) ;
#2000 = EDGE_LOOP ( 'NONE', ( #9896, #8367, #1939, #14550, #9331, #7410, #910, #10343, #14966, #2582, #3013, #9491, #9674, #4922, #5681, #7893, #3016, #725, #11089, #13395, #7140, #11239, #8234, #12200, #11532, #11838, #2033, #6383, #4052, #1090, #2136, #4221, #1403, #5996, #11920, #11963, #892, #9564, #11403, #13099, #8619, #4823, #10537, #9188, #11351, #5824, #8576, #14215, #8041, #13149, #4145, #2623, #10185, #2845, #13325, #2439, #5132, #8048, #4508, #735, #13449, #6191, #10853, #5120, #14332, #8200, #9101, #7690, #12126, #10347, #15073, #9430, #11895, #2736, #4037, #6352, #1983, #3068, #10997, #6871, #5073, #8581, #14641, #2342, #2309, #5128, #2095, #9777, #8804, #15069, #7631, #2847, #2718, #5362, #13193, #9829, #13079, #5922, #5765, #773, #659, #11259, #12675, #262, #6089, #14810, #11593, #4195, #4465, #12949, #3043, #2684, #9023, #9785, #533, #10287, #13024, #6773, #10364, #4152, #4871, #6630, #10079, #6422, #3558, #10272, #8950, #9508, #1188, #905, #1852, #8740, #4243, #2080, #5034, #875, #3821, #1796, #8258, #10403, #6297, #9755, #7143, #2703, #12716, #10408, #8785, #7334, #257, #6107, #6449, #11724, #2905, #14417, #4111, #9008, #14386, #5234, #12014, #10038, #85, #10520, #5979, #11834, #14681, #11645, #4031, #1573, #11487, #11188, #6424, #5512, #6611, #1167, #5713, #7487, #1499, #5859, #3710, #1461, #9409, #1795 ) ) ;
#1999 = CARTESIAN_POINT ( 'NONE',  ( -9.251715890255169938, -8.391880844292892050, 56.85231026484398598 ) ) ;
#2001 = ORIENTED_EDGE ( 'NONE', *, *, #476, .T. ) ;
#2002 = DIRECTION ( 'NONE',  ( 0.5975035461963189576, 0.8018662683283437342, 0.000000000000000000 ) ) ;
#2003 = ORIENTED_EDGE ( 'NONE', *, *, #4497, .T. ) ;
#2004 = CIRCLE ( 'NONE', #3705, 9.974999999999999645 ) ;
#2005 = CARTESIAN_POINT ( 'NONE',  ( -5.499699860811004370, -46.50737899243799944, 44.50231026484399877 ) ) ;
#2006 = CARTESIAN_POINT ( 'NONE',  ( -7.499699860810999041, -19.50737899243799589, 60.84879442494580104 ) ) ;
#2007 = CARTESIAN_POINT ( 'NONE',  ( -5.923714809816988058, -16.30043024566306187, 54.00231026484400587 ) ) ;
#2008 = AXIS2_PLACEMENT_3D ( 'NONE', #7616, #10918, #12298 ) ;
#2009 = CIRCLE ( 'NONE', #6637, 37.50000000000000000 ) ;
#2010 = DIRECTION ( 'NONE',  ( -8.018662683283439195E-16, 5.975035461963190001E-16, 1.000000000000000000 ) ) ;
#2011 = PRODUCT ( 'Indexable Carbide Insert', 'Indexable Carbide Insert', '', ( #12530 ) ) ;
#2012 = ADVANCED_FACE ( 'NONE', ( #5620 ), #2416, .T. ) ;
#2013 = AXIS2_PLACEMENT_3D ( 'NONE', #14988, #13994, #13770 ) ;
#2014 = DIRECTION ( 'NONE',  ( 0.04695496274984587576, 0.9988970074402868660, -5.591929034707467802E-16 ) ) ;
#2015 = ORIENTED_EDGE ( 'NONE', *, *, #9387, .T. ) ;
#2016 = CARTESIAN_POINT ( 'NONE',  ( 16.55725115840230544, -23.76580534705618675, 43.67529649635483224 ) ) ;
#2017 = VERTEX_POINT ( 'NONE', #8215 ) ;
#2018 = CARTESIAN_POINT ( 'NONE',  ( 2.500300139188999182, -42.00737899243800655, 52.39987856403599409 ) ) ;
#2019 = ORIENTED_EDGE ( 'NONE', *, *, #11672, .T. ) ;
#2020 = VERTEX_POINT ( 'NONE', #2341 ) ;
#2021 = CYLINDRICAL_SURFACE ( 'NONE', #11768, 22.99999999999999645 ) ;
#2022 = ORIENTED_EDGE ( 'NONE', *, *, #10197, .F. ) ;
#2023 = CARTESIAN_POINT ( 'NONE',  ( -7.758527451664999575, -46.50737899243799944, -5.497689735156000346 ) ) ;
#2024 = AXIS2_PLACEMENT_3D ( 'NONE', #4230, #2704, #8583 ) ;
#2025 = AXIS2_PLACEMENT_3D ( 'NONE', #2302, #10326, #4523 ) ;
#2026 = DIRECTION ( 'NONE',  ( 0.000000000000000000, 0.000000000000000000, 1.000000000000000000 ) ) ;
#2027 = DIRECTION ( 'NONE',  ( 0.000000000000000000, 1.000000000000000000, 1.224646799147350002E-16 ) ) ;
#2028 = CARTESIAN_POINT ( 'NONE',  ( 14.70436407088162767, -26.54712960475821149, 1.986671089746397056 ) ) ;
#2029 = CARTESIAN_POINT ( 'NONE',  ( -25.49969986081099904, -13.50737899243799944, 6.712064221500998684 ) ) ;
#2030 = EDGE_CURVE ( 'NONE', #2942, #6582, #7059, .T. ) ;
#2032 = CARTESIAN_POINT ( 'NONE',  ( -15.49969986081099904, 64.39262100756199914, 24.21206422150100579 ) ) ;
#2031 = DIRECTION ( 'NONE',  ( 1.054621095516909827E-16, 0.000000000000000000, -1.000000000000000000 ) ) ;
#2033 = ORIENTED_EDGE ( 'NONE', *, *, #14429, .T. ) ;
#2034 = CARTESIAN_POINT ( 'NONE',  ( -7.753733168396166775, -46.50737899243799944, 42.00231026484399166 ) ) ;
#2035 = PLANE ( 'NONE',  #8386 ) ;
#2036 = ORIENTED_EDGE ( 'NONE', *, *, #2242, .T. ) ;
#2037 = ORIENTED_EDGE ( 'NONE', *, *, #7170, .F. ) ;
#2038 = FACE_OUTER_BOUND ( 'NONE', #6532, .T. ) ;
#2039 = AXIS2_PLACEMENT_3D ( 'NONE', #12387, #9930, #11161 ) ;
#2040 = EDGE_CURVE ( 'NONE', #13214, #1579, #15053, .T. ) ;
#2041 = VECTOR ( 'NONE', #9536, 1000.000000000000000 ) ;
#2042 = CARTESIAN_POINT ( 'NONE',  ( -100.5053766806731090, -107.1622034095863825, -6.087689735156085469 ) ) ;
#2043 = DIRECTION ( 'NONE',  ( 0.000000000000000000, 0.000000000000000000, 1.000000000000000000 ) ) ;
#2044 = ORIENTED_EDGE ( 'NONE', *, *, #4686, .T. ) ;
#2045 = CARTESIAN_POINT ( 'NONE',  ( -15.49969986081099904, -27.00737899243800300, -5.497689735156002122 ) ) ;
#2046 = CARTESIAN_POINT ( 'NONE',  ( -22.33089034576175180, -8.323646113680169378, 57.00231026484397745 ) ) ;
#2047 = PRODUCT_CONTEXT ( 'NONE', #9961, 'mechanical' ) ;
#2048 = AXIS2_PLACEMENT_3D ( 'NONE', #3286, #7934, #10469 ) ;
#2049 = CARTESIAN_POINT ( 'NONE',  ( -7.553613233656760073, -48.84439576093267021, 20.40192502283242959 ) ) ;
#2050 = CARTESIAN_POINT ( 'NONE',  ( -8.639554752241616953, -9.247137322136806503, 56.85231026484400019 ) ) ;
#2051 = EDGE_CURVE ( 'NONE', #4847, #13967, #11515, .T. ) ;
#2052 = DIRECTION ( 'NONE',  ( -0.1908089953765463587, 0.5346324819374547177, 0.8232618274527189195 ) ) ;
#2053 = ORIENTED_EDGE ( 'NONE', *, *, #12377, .T. ) ;
#2054 = CARTESIAN_POINT ( 'NONE',  ( -15.18865579839852487, -94.57871019452736050, -0.1345408968949149964 ) ) ;
#2055 = EDGE_CURVE ( 'NONE', #5382, #947, #7156, .T. ) ;
#2056 = CARTESIAN_POINT ( 'NONE',  ( -7.509061791769728877, -44.91935217387478474, -3.566842261944418890 ) ) ;
#2057 = AXIS2_PLACEMENT_3D ( 'NONE', #6307, #10987, #5390 ) ;
#2058 = LINE ( 'NONE', #1206, #13789 ) ;
#2059 = EDGE_CURVE ( 'NONE', #11803, #2347, #9290, .T. ) ;
#2060 = VERTEX_POINT ( 'NONE', #5917 ) ;
#2062 = ORIENTED_EDGE ( 'NONE', *, *, #5233, .T. ) ;
#2061 = CARTESIAN_POINT ( 'NONE',  ( -15.16333526000375365, -10.64029123852185776, 56.89875687425070794 ) ) ;
#2063 = ORIENTED_EDGE ( 'NONE', *, *, #12396, .F. ) ;
#2064 = AXIS2_PLACEMENT_3D ( 'NONE', #9708, #13386, #10930 ) ;
#2065 = DIRECTION ( 'NONE',  ( 8.018662683283438208E-16, -5.975035461963189015E-16, -1.000000000000000000 ) ) ;
#2066 = CARTESIAN_POINT ( 'NONE',  ( -11.94576515372786751, -51.69378783610798678, 56.83668549888485444 ) ) ;
#2067 = ADVANCED_FACE ( 'NONE', ( #9062 ), #3482, .F. ) ;
#2068 = PLANE ( 'NONE',  #2985 ) ;
#2069 = LINE ( 'NONE', #5502, #850 ) ;
#2070 = CARTESIAN_POINT ( 'NONE',  ( -5.636125951381724342, -11.86928948430367114, 60.39167800444882062 ) ) ;
#2071 = COLOUR_RGB ( '', 0.08235294, 0.09019608, 0.10196078) ;
#2072 = CARTESIAN_POINT ( 'NONE',  ( 2.500300139188999182, -46.50737899243799944, 19.50231026484399877 ) ) ;
#2073 = EDGE_CURVE ( 'NONE', #6681, #5621, #5936, .T. ) ;
#2074 = DIRECTION ( 'NONE',  ( 1.000000000000000000, 1.000000000000000078E-15, 0.000000000000000000 ) ) ;
#2075 = FACE_OUTER_BOUND ( 'NONE', #2759, .T. ) ;
#2076 = ORIENTED_EDGE ( 'NONE', *, *, #5249, .T. ) ;
#2077 = DIRECTION ( 'NONE',  ( -8.018662683283438208E-16, 5.975035461963189015E-16, 1.000000000000000000 ) ) ;
#2078 = CARTESIAN_POINT ( 'NONE',  ( -18.43409448121630945, -5.984417261063049942, 57.00231026484397745 ) ) ;
#2080 = ORIENTED_EDGE ( 'NONE', *, *, #2193, .F. ) ;
#2079 = FACE_OUTER_BOUND ( 'NONE', #3086, .T. ) ;
#2081 = ORIENTED_EDGE ( 'NONE', *, *, #5399, .F. ) ;
#2082 = FACE_OUTER_BOUND ( 'NONE', #10563, .T. ) ;
#2083 = ORIENTED_EDGE ( 'NONE', *, *, #4124, .T. ) ;
#2084 = CARTESIAN_POINT ( 'NONE',  ( -18.09969986081091164, -109.9722034095862995, -10.19792577984107318 ) ) ;
#2085 = VECTOR ( 'NONE', #9418, 1000.000000000000000 ) ;
#2086 = PRODUCT_RELATED_PRODUCT_CATEGORY ( 'part', '', ( #11171 ) ) ;
#2087 = ADVANCED_FACE ( 'NONE', ( #8140 ), #12673, .T. ) ;
#2088 = CARTESIAN_POINT ( 'NONE',  ( -20.84918524500973191, -107.1622034095862972, -5.012689735156006243 ) ) ;
#2089 =( NAMED_UNIT ( * ) PLANE_ANGLE_UNIT ( ) SI_UNIT ( $, .RADIAN. ) );
#2090 = ORIENTED_EDGE ( 'NONE', *, *, #2040, .T. ) ;
#2091 = CARTESIAN_POINT ( 'NONE',  ( -7.867938255526238933, -47.21659244687199219, -7.899326032359201832 ) ) ;
#2092 = CARTESIAN_POINT ( 'NONE',  ( -18.08104095141683487, -52.09767164165551634, -17.91190622590529102 ) ) ;
#2093 = VERTEX_POINT ( 'NONE', #13961 ) ;
#2094 = DIRECTION ( 'NONE',  ( 8.018662683283438208E-16, -5.975035461963189015E-16, -1.000000000000000000 ) ) ;
#2095 = ORIENTED_EDGE ( 'NONE', *, *, #12824, .T. ) ;
#2096 = FACE_OUTER_BOUND ( 'NONE', #1893, .T. ) ;
#2097 = ORIENTED_EDGE ( 'NONE', *, *, #9986, .F. ) ;
#2098 = ORIENTED_EDGE ( 'NONE', *, *, #2319, .F. ) ;
#2099 = CARTESIAN_POINT ( 'NONE',  ( 2.598755596215367447, -41.01804242336424267, 52.34582402777507326 ) ) ;
#2100 = ORIENTED_EDGE ( 'NONE', *, *, #9855, .F. ) ;
#2101 = CARTESIAN_POINT ( 'NONE',  ( -7.264457220180047692, -15.89840986842769333, 56.85231026484400019 ) ) ;
#2102 = ADVANCED_FACE ( 'NONE', ( #5696 ), #4556, .F. ) ;
#2103 = EDGE_CURVE ( 'NONE', #11708, #8808, #7400, .T. ) ;
#2104 = CIRCLE ( 'NONE', #4796, 9.974999999999999645 ) ;
#2105 = DIRECTION ( 'NONE',  ( -0.9805849309054471830, -0.1960948578651655061, -6.691306063588582470E-16 ) ) ;
#2106 = CARTESIAN_POINT ( 'NONE',  ( -15.49969986081092088, -13.50737899243822504, 56.85231026484398598 ) ) ;
#2107 = CIRCLE ( 'NONE', #14801, 1.249999999999999778 ) ;
#2108 = CARTESIAN_POINT ( 'NONE',  ( -7.509081646391243758, -44.91911869546537162, 21.43296569163635112 ) ) ;
#2110 = LINE ( 'NONE', #11436, #1911 ) ;
#2109 = DIRECTION ( 'NONE',  ( 0.5975035461963188466, 0.8018662683283437342, 0.000000000000000000 ) ) ;
#2111 = ORIENTED_EDGE ( 'NONE', *, *, #8347, .F. ) ;
#2112 = CARTESIAN_POINT ( 'NONE',  ( -15.61203582817000068, -106.2173407584721616, -5.758565883178085265 ) ) ;
#2113 = CARTESIAN_POINT ( 'NONE',  ( -16.08583582846909721, -17.97886954641662527, -13.28448150985099296 ) ) ;
#2114 = VERTEX_POINT ( 'NONE', #12124 ) ;
#2115 = ORIENTED_EDGE ( 'NONE', *, *, #8226, .T. ) ;
#2116 = DIRECTION ( 'NONE',  ( -1.000000000000000000, -1.000000000000000078E-15, 0.000000000000000000 ) ) ;
#2117 = CARTESIAN_POINT ( 'NONE',  ( -23.49969986081100259, -44.24330093701085787, 56.13904046828874073 ) ) ;
#2118 = ORIENTED_EDGE ( 'NONE', *, *, #3346, .F. ) ;
#2119 = PLANE ( 'NONE',  #11019 ) ;
#2120 = EDGE_CURVE ( 'NONE', #14475, #11896, #13290, .T. ) ;
#2121 = DIRECTION ( 'NONE',  ( 0.000000000000000000, 0.1872998510044521503, 0.9823027872370667657 ) ) ;
#2122 = DIRECTION ( 'NONE',  ( -0.8885476655824650072, -0.4587843131450243805, -4.383711467890778149E-16 ) ) ;
#2123 = CIRCLE ( 'NONE', #12879, 8.000000000000000000 ) ;
#2124 = DIRECTION ( 'NONE',  ( -8.018662683283438208E-16, 5.975035461963189015E-16, 1.000000000000000000 ) ) ;
#2125 = DIRECTION ( 'NONE',  ( -0.01206535623791937448, -0.9999272109403024578, 5.877852522924727828E-16 ) ) ;
#2126 = VERTEX_POINT ( 'NONE', #1494 ) ;
#2127 = DIRECTION ( 'NONE',  ( -1.000000000000000000, -1.000000000000000078E-15, -1.000000000000000078E-15 ) ) ;
#2128 = CARTESIAN_POINT ( 'NONE',  ( -36.87432072752655898, 5.512834891065107712, 29.00861863932625795 ) ) ;
#2129 = B_SPLINE_CURVE_WITH_KNOTS ( 'NONE', 3,
 ( #11939, #9713, #7409, #1456, #6103, #12092 ),
 .UNSPECIFIED., .F., .F.,
 ( 4, 2, 4 ),
 ( 0.7880782322772789117, 0.8940391161386394003, 1.000000000000000000 ),
 .UNSPECIFIED. ) ;
#2130 = DIRECTION ( 'NONE',  ( 0.000000000000000000, -1.000000000000000000, -1.224646799147350002E-16 ) ) ;
#2131 = CIRCLE ( 'NONE', #1633, 3.000000000000002665 ) ;
#2132 = DIRECTION ( 'NONE',  ( 0.000000000000000000, 9.251858538542971581E-17, -1.000000000000000000 ) ) ;
#2133 = VECTOR ( 'NONE', #2205, 1000.000000000000000 ) ;
#2134 = VERTEX_POINT ( 'NONE', #1420 ) ;
#2135 = CARTESIAN_POINT ( 'NONE',  ( -7.753733168396170328, -46.50737899243799944, 47.00231026484399877 ) ) ;
#2136 = ORIENTED_EDGE ( 'NONE', *, *, #11513, .F. ) ;
#2137 = B_SPLINE_CURVE_WITH_KNOTS ( 'NONE', 3,
 ( #885, #6678, #5836, #15102, #14038, #5613, #5691, #6750, #961, #15027, #10514, #4630, #4477, #9203, #2108, #3477, #8133, #2259, #6971, #42, #4709, #9056, #2182 ),
 .UNSPECIFIED., .F., .F.,
 ( 4, 2, 2, 2, 2, 2, 2, 2, 1, 1, 1, 2, 4 ),
 ( 0.1210918566152707487, 0.1627725786707973910, 0.2044533007263240609, 0.2878147448373775674, 0.4545376330594838032, 0.5378990771705385310, 0.5587394381983011860, 0.5613444833267742240, 0.5639495284552472620, 0.5691596187121935602, 0.5795797992260810494, 0.6212605212816443290, 0.7879834095039132125 ),
 .UNSPECIFIED. ) ;
#2138 = CARTESIAN_POINT ( 'NONE',  ( -23.54151295824578227, -12.77219731018227300, 56.85231026484398598 ) ) ;
#2139 = CARTESIAN_POINT ( 'NONE',  ( -11.48672836878686532, -51.44777436587664710, 56.78953867381472520 ) ) ;
#2140 = AXIS2_PLACEMENT_3D ( 'NONE', #10612, #216, #11994 ) ;
#2141 = EDGE_CURVE ( 'NONE', #5522, #4357, #99, .T. ) ;
#2142 = CARTESIAN_POINT ( 'NONE',  ( -14.00164528647249007, -5.572553380472728968, 57.00231026484397745 ) ) ;
#2143 = CARTESIAN_POINT ( 'NONE',  ( -15.49969986081091200, -13.50737899243823215, 48.00231026484398456 ) ) ;
#2144 = EDGE_CURVE ( 'NONE', #5192, #10261, #6221, .T. ) ;
#2145 = DIRECTION ( 'NONE',  ( -1.000000000000000000, 0.000000000000000000, 0.000000000000000000 ) ) ;
#2146 = CARTESIAN_POINT ( 'NONE',  ( -15.49969986081092088, -13.50737899243822504, 57.00231026484397745 ) ) ;
#2147 = AXIS2_PLACEMENT_3D ( 'NONE', #6754, #11438, #6603 ) ;
#2148 = CARTESIAN_POINT ( 'NONE',  ( -5.596483669297570351, -12.31283553816471432, 56.85231026484400019 ) ) ;
#2149 = EDGE_CURVE ( 'NONE', #5040, #15014, #8290, .T. ) ;
#2150 = CARTESIAN_POINT ( 'NONE',  ( -19.06972223273333711, -21.85101071153832919, 56.85231026484400019 ) ) ;
#2151 = VECTOR ( 'NONE', #2496, 1000.000000000000000 ) ;
#2152 = VERTEX_POINT ( 'NONE', #8598 ) ;
#2153 = CARTESIAN_POINT ( 'NONE',  ( 18.53245405280428315, -27.23732813736695846, 39.96206422150099513 ) ) ;
#2154 = ORIENTED_EDGE ( 'NONE', *, *, #13626, .F. ) ;
#2155 = FILL_AREA_STYLE_COLOUR ( '', #11648 ) ;
#2157 = ORIENTED_EDGE ( 'NONE', *, *, #13527, .F. ) ;
#2156 = DIRECTION ( 'NONE',  ( 0.000000000000000000, 1.000000000000000000, 0.000000000000000000 ) ) ;
#2158 = ORIENTED_EDGE ( 'NONE', *, *, #9814, .T. ) ;
#2159 = CARTESIAN_POINT ( 'NONE',  ( -21.79090396836353705, -19.33464257641254136, 57.00231026484397745 ) ) ;
#2160 = CARTESIAN_POINT ( 'NONE',  ( -15.83606446161809522, -16.37446674635458166, 56.75231026484397745 ) ) ;
#2161 = ORIENTED_EDGE ( 'NONE', *, *, #7090, .T. ) ;
#2162 = CARTESIAN_POINT ( 'NONE',  ( 0.8918609567539013128, -25.75737899243799944, -17.99768973515599768 ) ) ;
#2163 = ADVANCED_FACE ( 'NONE', ( #11978 ), #4939, .F. ) ;
#2164 = EDGE_CURVE ( 'NONE', #13375, #2383, #1391, .T. ) ;
#2165 = AXIS2_PLACEMENT_3D ( 'NONE', #11467, #12933, #8243 ) ;
#2166 = CYLINDRICAL_SURFACE ( 'NONE', #10265, 2.000000000000001776 ) ;
#2167 = ORIENTED_EDGE ( 'NONE', *, *, #5276, .F. ) ;
#2168 = DIRECTION ( 'NONE',  ( -8.018662683283438208E-16, 5.975035461963189015E-16, 1.000000000000000000 ) ) ;
#2169 = ORIENTED_EDGE ( 'NONE', *, *, #12328, .F. ) ;
#2170 = CARTESIAN_POINT ( 'NONE',  ( 18.44256572617712209, -25.88025075299395894, 40.15519541060486830 ) ) ;
#2171 = ORIENTED_EDGE ( 'NONE', *, *, #12744, .F. ) ;
#2172 = AXIS2_PLACEMENT_3D ( 'NONE', #13448, #7613, #13368 ) ;
#2173 = CARTESIAN_POINT ( 'NONE',  ( -20.59651154950486784, -18.41489981358536809, 56.85231026484398598 ) ) ;
#2174 = ORIENTED_EDGE ( 'NONE', *, *, #3341, .T. ) ;
#2175 = VERTEX_POINT ( 'NONE', #7369 ) ;
#2176 = ORIENTED_EDGE ( 'NONE', *, *, #14828, .T. ) ;
#2177 = CARTESIAN_POINT ( 'NONE',  ( -15.49969986081091200, -13.50737899243823037, 48.00231026484398456 ) ) ;
#2178 = EDGE_CURVE ( 'NONE', #1908, #13484, #91, .T. ) ;
#2179 = VECTOR ( 'NONE', #4222, 1000.000000000000000 ) ;
#2180 = PLANE ( 'NONE',  #18 ) ;
#2181 = CARTESIAN_POINT ( 'NONE',  ( -15.49969986081099904, -37.00737899243799944, 19.50231026484399877 ) ) ;
#2182 = CARTESIAN_POINT ( 'NONE',  ( -7.501950027729723303, -44.50597529135383468, 20.99749114769749880 ) ) ;
#2184 = CARTESIAN_POINT ( 'NONE',  ( 7.200737182676100190, 4.873818854045000037, 27.91208557747711083 ) ) ;
#2183 = LINE ( 'NONE', #4552, #10835 ) ;
#2185 = VERTEX_POINT ( 'NONE', #202 ) ;
#2186 = CARTESIAN_POINT ( 'NONE',  ( -21.79090396836353705, -19.33464257641254136, 56.85231026484398598 ) ) ;
#2187 = AXIS2_PLACEMENT_3D ( 'NONE', #11488, #6880, #13860 ) ;
#2188 = CARTESIAN_POINT ( 'NONE',  ( -16.66704480552753509, -17.86341950268894152, -13.27088927653592521 ) ) ;
#2189 = ORIENTED_EDGE ( 'NONE', *, *, #13571, .F. ) ;
#2190 = VECTOR ( 'NONE', #12683, 1000.000000000000000 ) ;
#2191 = ORIENTED_EDGE ( 'NONE', *, *, #9300, .F. ) ;
#2192 = DIRECTION ( 'NONE',  ( -1.000000000000000000, 0.000000000000000000, 0.000000000000000000 ) ) ;
#2193 = EDGE_CURVE ( 'NONE', #13665, #3051, #11894, .T. ) ;
#2194 = DIRECTION ( 'NONE',  ( -0.4491835085186243748, -0.8934395198752397294, 1.736481776669299976E-16 ) ) ;
#2195 = FACE_OUTER_BOUND ( 'NONE', #9256, .T. ) ;
#2196 = VERTEX_POINT ( 'NONE', #14192 ) ;
#2197 = DIRECTION ( 'NONE',  ( 8.018662683283438208E-16, -5.975035461963189015E-16, -1.000000000000000000 ) ) ;
#2198 = DIRECTION ( 'NONE',  ( 1.000000000000000000, 1.201369187114119994E-15, 9.616040805000176517E-16 ) ) ;
#2199 = VECTOR ( 'NONE', #9977, 1000.000000000000000 ) ;
#2200 = CARTESIAN_POINT ( 'NONE',  ( -20.54757852167729837, -19.81012014412530320, 57.00231026484397745 ) ) ;
#2201 = LINE ( 'NONE', #8156, #6447 ) ;
#2203 = ORIENTED_EDGE ( 'NONE', *, *, #4234, .F. ) ;
#2202 = AXIS2_PLACEMENT_3D ( 'NONE', #5298, #419, #10029 ) ;
#2204 = CARTESIAN_POINT ( 'NONE',  ( -14.81665476263932213, -93.72685551323446873, -0.1697857866622040635 ) ) ;
#2205 = DIRECTION ( 'NONE',  ( 0.03489949670249904018, 0.9993908270190957621, 3.917345239535707520E-17 ) ) ;
#2206 = DIRECTION ( 'NONE',  ( -1.000000000000000000, 0.000000000000000000, 0.000000000000000000 ) ) ;
#2207 = ADVANCED_FACE ( 'NONE', ( #9753 ), #13057, .F. ) ;
#2208 = CARTESIAN_POINT ( 'NONE',  ( -10.95221305062249684, -4.629260458021021485, 56.85231026484398598 ) ) ;
#2209 = EDGE_LOOP ( 'NONE', ( #1296, #13653, #4393, #3487 ) ) ;
#2210 = ADVANCED_FACE ( 'NONE', ( #13284 ), #4868, .T. ) ;
#2211 = PLANE ( 'NONE',  #12068 ) ;
#2212 = VERTEX_POINT ( 'NONE', #13134 ) ;
#2213 = DIRECTION ( 'NONE',  ( -8.018662683283438208E-16, 5.975035461963189015E-16, 1.000000000000000000 ) ) ;
#2214 = CARTESIAN_POINT ( 'NONE',  ( -1.508527451664999575, -46.50737899243799234, -3.997689735156000790 ) ) ;
#2215 = CARTESIAN_POINT ( 'NONE',  ( -16.34789837066771767, -3.568506607309358092, 54.00231026484397745 ) ) ;
#2216 = VECTOR ( 'NONE', #12876, 999.9999999999998863 ) ;
#2217 = DIRECTION ( 'NONE',  ( 1.000000000000000000, 1.000000000000000078E-15, 0.000000000000000000 ) ) ;
#2218 = CARTESIAN_POINT ( 'NONE',  ( -7.512805849530849400, -44.04964101872670312, 19.04457229113268113 ) ) ;
#2219 = CARTESIAN_POINT ( 'NONE',  ( -13.57551609484869282, -3.719726473329895811, 57.00231026484397745 ) ) ;
#2220 = CARTESIAN_POINT ( 'NONE',  ( -10.84210729886283531, -6.910555398701176522, 56.85231026484398598 ) ) ;
#2221 = CARTESIAN_POINT ( 'NONE',  ( -16.41401162527548507, -4.478243707298169340, 57.00231026484397745 ) ) ;
#2222 = LINE ( 'NONE', #4371, #4233 ) ;
#2223 = EDGE_CURVE ( 'NONE', #7254, #11993, #1640, .T. ) ;
#2224 = ORIENTED_EDGE ( 'NONE', *, *, #8966, .F. ) ;
#2225 = FACE_OUTER_BOUND ( 'NONE', #8148, .T. ) ;
#2226 = ORIENTED_EDGE ( 'NONE', *, *, #13237, .T. ) ;
#2228 = ORIENTED_EDGE ( 'NONE', *, *, #14180, .F. ) ;
#2227 = CARTESIAN_POINT ( 'NONE',  ( -15.49969986081099904, -26.50737899243800300, 19.50231026484400232 ) ) ;
#2229 = EDGE_LOOP ( 'NONE', ( #10517, #10508, #4637, #14470 ) ) ;
#2230 = EDGE_CURVE ( 'NONE', #4277, #13407, #13346, .T. ) ;
#2231 = FACE_OUTER_BOUND ( 'NONE', #9448, .T. ) ;
#2232 = ORIENTED_EDGE ( 'NONE', *, *, #6822, .T. ) ;
#2233 = CARTESIAN_POINT ( 'NONE',  ( -15.49969986081099904, -32.00737899243799944, 24.21206422150100224 ) ) ;
#2234 = CARTESIAN_POINT ( 'NONE',  ( -19.51793069539949599, -6.502732608789604463, 57.00231026484397745 ) ) ;
#2235 = VECTOR ( 'NONE', #8892, 1000.000000000000000 ) ;
#2236 = DIRECTION ( 'NONE',  ( -8.018662683283438208E-16, 5.975035461963189015E-16, 1.000000000000000000 ) ) ;
#2237 = EDGE_LOOP ( 'NONE', ( #14384, #10976, #3945, #8743 ) ) ;
#2238 = CARTESIAN_POINT ( 'NONE',  ( -23.49969986081100615, -44.76879304137393234, -17.13441993860073254 ) ) ;
#2239 = ADVANCED_FACE ( 'NONE', ( #10826 ), #6140, .F. ) ;
#2240 = ORIENTED_EDGE ( 'NONE', *, *, #8119, .F. ) ;
#2241 = CARTESIAN_POINT ( 'NONE',  ( -15.49969986081099904, 2.992621007562000557, -3.787935778499000428 ) ) ;
#2242 = EDGE_CURVE ( 'NONE', #10422, #14849, #6514, .T. ) ;
#2243 = EDGE_LOOP ( 'NONE', ( #14326, #12234, #4361, #8195 ) ) ;
#2244 = DIRECTION ( 'NONE',  ( 0.000000000000000000, -1.000000000000000000, -1.224646799147350002E-16 ) ) ;
#2245 = VERTEX_POINT ( 'NONE', #6444 ) ;
#2246 = ORIENTED_EDGE ( 'NONE', *, *, #7374, .F. ) ;
#2247 = VECTOR ( 'NONE', #10805, 1000.000000000000114 ) ;
#2248 = EDGE_CURVE ( 'NONE', #17, #10747, #2104, .T. ) ;
#2249 = CARTESIAN_POINT ( 'NONE',  ( -9.452813543643186378, -20.27468391147722926, 57.00231026484399166 ) ) ;
#2250 = ORIENTED_EDGE ( 'NONE', *, *, #10858, .T. ) ;
#2251 = CARTESIAN_POINT ( 'NONE',  ( 13.85920135429429934, -27.00737899243800300, 40.71206422150099513 ) ) ;
#2252 = ADVANCED_FACE ( 'NONE', ( #13500 ), #8669, .T. ) ;
#2253 = CARTESIAN_POINT ( 'NONE',  ( -18.09969986081099336, -110.0345591146135860, -9.886379190557276431 ) ) ;
#2254 = AXIS2_PLACEMENT_3D ( 'NONE', #5292, #4071, #13196 ) ;
#2255 = CARTESIAN_POINT ( 'NONE',  ( -15.49969986081099904, 10.68321993080349763, 24.21206422150099868 ) ) ;
#2256 = VECTOR ( 'NONE', #14650, 1000.000000000000000 ) ;
#2257 = VECTOR ( 'NONE', #6759, 1000.000000000000114 ) ;
#2258 = VECTOR ( 'NONE', #11093, 1000.000000000000114 ) ;
#2259 = CARTESIAN_POINT ( 'NONE',  ( -7.508535857682161030, -44.90886896333648792, 21.42449717988529656 ) ) ;
#2261 = CARTESIAN_POINT ( 'NONE',  ( -23.36093307149983289, -11.66014798166512634, 56.85231026484398598 ) ) ;
#2260 = CARTESIAN_POINT ( 'NONE',  ( -10.96544185377836911, -6.825182173602284408, 57.00231026484397745 ) ) ;
#2262 = ORIENTED_EDGE ( 'NONE', *, *, #7855, .T. ) ;
#2263 = CARTESIAN_POINT ( 'NONE',  ( -7.499699860810999041, -44.50737899243799944, 43.00231026484400587 ) ) ;
#2264 = EDGE_CURVE ( 'NONE', #12036, #10807, #1794, .T. ) ;
#2265 = CARTESIAN_POINT ( 'NONE',  ( -15.79357609952228714, -18.00737899243800300, -13.28793577849899066 ) ) ;
#2266 = B_SPLINE_CURVE_WITH_KNOTS ( 'NONE', 3,
 ( #13174, #6030, #4909, #397, #9716, #13248, #7411, #14605, #10078, #13393, #761, #12163, #8708, #1678, #2757, #11087, #7703, #5197, #14534, #13466, #8562, #610, #14456, #6407, #1831, #9866, #2973, #6258, #12094, #12239, #8783, #2903, #468, #6477, #1605 ),
 .UNSPECIFIED., .F., .F.,
 ( 4, 2, 2, 2, 2, 2, 2, 2, 2, 1, 1, 2, 2, 2, 1, 1, 1, 2, 2, 4 ),
 ( 0.000000000000000000, 0.06249999999999285294, 0.09374999999998914757, 0.1249999999999854283, 0.1874999999999780176, 0.2187499999999731326, 0.2499999999999682476, 0.3749999999999460432, 0.4374999999999342193, 0.4687499999999275024, 0.4843749999999235056, 0.4921874999999215072, 0.4999999999999195088, 0.6249999999999151790, 0.6874999999999131806, 0.7187499999999130695, 0.7343749999999139577, 0.7421874999999155120, 0.7499999999999169553, 1.000000000000000000 ),
 .UNSPECIFIED. ) ;
#2267 = ORIENTED_EDGE ( 'NONE', *, *, #7549, .T. ) ;
#2268 = EDGE_LOOP ( 'NONE', ( #11162, #2666, #11805, #3888 ) ) ;
#2269 = DIRECTION ( 'NONE',  ( 0.000000000000000000, 0.000000000000000000, 1.000000000000000000 ) ) ;
#2270 = ADVANCED_FACE ( 'NONE', ( #10037 ), #5237, .T. ) ;
#2271 = DIRECTION ( 'NONE',  ( 0.000000000000000000, 0.000000000000000000, -1.000000000000000000 ) ) ;
#2272 = AXIS2_PLACEMENT_3D ( 'NONE', #4471, #9197, #9126 ) ;
#2273 = CARTESIAN_POINT ( 'NONE',  ( -15.49969986081099371, -36.50737899243799944, -17.99768973515599768 ) ) ;
#2274 = ORIENTED_EDGE ( 'NONE', *, *, #4328, .F. ) ;
#2275 = DIRECTION ( 'NONE',  ( -1.000000000000000000, 0.000000000000000000, 0.000000000000000000 ) ) ;
#2276 = CARTESIAN_POINT ( 'NONE',  ( -7.758527451664997798, -48.50737899243800655, -5.497689735156000346 ) ) ;
#2277 = ITEM_DEFINED_TRANSFORMATION ( 'NONE', 'NONE', #10229,  #6789 ) ;
#2278 = EDGE_CURVE ( 'NONE', #10020, #234, #720, .T. ) ;
#2279 = PLANE ( 'NONE',  #10446 ) ;
#2280 = VECTOR ( 'NONE', #7101, 1000.000000000000227 ) ;
#2281 = DIRECTION ( 'NONE',  ( -0.8599296884906622029, 0.5104125104779001498, -9.945218953682734920E-16 ) ) ;
#2282 = CARTESIAN_POINT ( 'NONE',  ( -15.49969986081099904, -107.1622034095870077, -6.087689735155999315 ) ) ;
#2283 = EDGE_LOOP ( 'NONE', ( #5368, #872, #7183, #13927 ) ) ;
#2284 = AXIS2_PLACEMENT_3D ( 'NONE', #962, #10209, #14882 ) ;
#2285 = CARTESIAN_POINT ( 'NONE',  ( -35.81405311550189197, 6.021066563906106950, 29.58511937964010485 ) ) ;
#2286 = CARTESIAN_POINT ( 'NONE',  ( -15.49969986081099904, 13.89262100756199736, 18.96206422150099868 ) ) ;
#2287 = CARTESIAN_POINT ( 'NONE',  ( -8.194314379747492438, -16.94868586237404529, 56.85231026484400019 ) ) ;
#2288 = VERTEX_POINT ( 'NONE', #6296 ) ;
#2289 = CARTESIAN_POINT ( 'NONE',  ( -3.508527451664997798, -48.23942980000687442, -5.497689735155999458 ) ) ;
#2290 = VERTEX_POINT ( 'NONE', #12426 ) ;
#2291 = PLANE ( 'NONE',  #9591 ) ;
#2292 = CARTESIAN_POINT ( 'NONE',  ( -15.49969986081094042, -85.00737899243800655, -5.497689735156000346 ) ) ;
#2293 = AXIS2_PLACEMENT_3D ( 'NONE', #8624, #10996, #2884 ) ;
#2294 = FACE_OUTER_BOUND ( 'NONE', #2000, .T. ) ;
#2295 = PRESENTATION_STYLE_ASSIGNMENT (( #10545 ) ) ;
#2296 = ADVANCED_FACE ( 'NONE', ( #2862 ), #4239, .T. ) ;
#2297 = CARTESIAN_POINT ( 'NONE',  ( -15.45180655762527699, -13.52173975529984418, 56.85231026484398598 ) ) ;
#2298 = AXIS2_PLACEMENT_3D ( 'NONE', #8828, #13512, #7682 ) ;
#2299 = DIRECTION ( 'NONE',  ( 1.000000000000000000, 1.201369187114119994E-15, 9.616040805000176517E-16 ) ) ;
#2300 = CARTESIAN_POINT ( 'NONE',  ( -38.49969986081099904, -37.00737899243799944, 49.12071670408379731 ) ) ;
#2301 = AXIS2_PLACEMENT_3D ( 'NONE', #13240, #14527, #1322 ) ;
#2302 = CARTESIAN_POINT ( 'NONE',  ( -5.499699860810998153, -46.50737899243799944, -5.497689735156003010 ) ) ;
#2303 = ORIENTED_EDGE ( 'NONE', *, *, #11629, .F. ) ;
#2304 = LINE ( 'NONE', #10555, #11760 ) ;
#2305 = ORIENTED_EDGE ( 'NONE', *, *, #9974, .F. ) ;
#2306 = DIRECTION ( 'NONE',  ( -1.000000000000000000, 0.000000000000000000, 0.000000000000000000 ) ) ;
#2308 = ORIENTED_EDGE ( 'NONE', *, *, #10566, .T. ) ;
#2307 = CARTESIAN_POINT ( 'NONE',  ( -18.72720981345337421, -4.041066102621154954, 61.57426170146454325 ) ) ;
#2309 = ORIENTED_EDGE ( 'NONE', *, *, #7, .F. ) ;
#2310 = PLANE ( 'NONE',  #2632 ) ;
#2311 = ORIENTED_EDGE ( 'NONE', *, *, #5771, .T. ) ;
#2312 = AXIS2_PLACEMENT_3D ( 'NONE', #7287, #14343, #11732 ) ;
#2313 = PLANE ( 'NONE',  #4874 ) ;
#2314 = CARTESIAN_POINT ( 'NONE',  ( -15.45180655762527699, -13.52173975529984418, 56.85231026484398598 ) ) ;
#2315 = VECTOR ( 'NONE', #7697, 1000.000000000000000 ) ;
#2316 = EDGE_CURVE ( 'NONE', #3863, #12839, #13376, .T. ) ;
#2317 = CARTESIAN_POINT ( 'NONE',  ( -6.405625242116718354, -17.60596799715946759, 56.85231026484400019 ) ) ;
#2318 = CARTESIAN_POINT ( 'NONE',  ( -28.78282149594069850, -31.14135358865350511, -123.9247733198440073 ) ) ;
#2319 = EDGE_CURVE ( 'NONE', #8706, #14042, #10975, .T. ) ;
#2320 = CARTESIAN_POINT ( 'NONE',  ( -23.48691887691489910, -45.03073692993354626, -17.13721805342403570 ) ) ;
#2321 = ORIENTED_EDGE ( 'NONE', *, *, #8050, .F. ) ;
#2322 = CARTESIAN_POINT ( 'NONE',  ( -11.45509117250411713, -15.50188834333807897, -13.06935246023203234 ) ) ;
#2323 = ORIENTED_EDGE ( 'NONE', *, *, #6147, .F. ) ;
#2324 = LINE ( 'NONE', #15090, #5063 ) ;
#2325 = EDGE_LOOP ( 'NONE', ( #7781, #5567, #10277, #9935 ) ) ;
#2326 = EDGE_LOOP ( 'NONE', ( #5933, #8488, #7665, #9351 ) ) ;
#2327 = VECTOR ( 'NONE', #13331, 1000.000000000000000 ) ;
#2328 = CARTESIAN_POINT ( 'NONE',  ( 3.941853951887407614, -38.49305635557872307, 51.56919050049003772 ) ) ;
#2329 = VERTEX_POINT ( 'NONE', #7740 ) ;
#2330 = CARTESIAN_POINT ( 'NONE',  ( -20.10554184627359220, -22.38357163673832417, 56.71843902453247921 ) ) ;
#2331 = EDGE_CURVE ( 'NONE', #12982, #3306, #7521, .T. ) ;
#2332 = FILL_AREA_STYLE_COLOUR ( '', #2071 ) ;
#2333 = DIRECTION ( 'NONE',  ( 1.000000000000000078E-15, -1.000000000000000000, 0.000000000000000000 ) ) ;
#2334 = EDGE_CURVE ( 'NONE', #11422, #6725, #14100, .T. ) ;
#2335 = EDGE_CURVE ( 'NONE', #700, #4277, #11126, .T. ) ;
#2336 = CARTESIAN_POINT ( 'NONE',  ( 6.045543233663400073, 20.99262100756200056, 32.26206422150099939 ) ) ;
#2338 = DIRECTION ( 'NONE',  ( -0.4895147004624045839, 0.8719950447285823580, -9.135454576426008610E-16 ) ) ;
#2337 = CARTESIAN_POINT ( 'NONE',  ( -20.61203582816999713, -107.1622034095870077, -6.087689735156005533 ) ) ;
#2339 = ORIENTED_EDGE ( 'NONE', *, *, #1951, .T. ) ;
#2340 = DIRECTION ( 'NONE',  ( 0.5975035461963189576, 0.8018662683283437342, 0.000000000000000000 ) ) ;
#2341 = CARTESIAN_POINT ( 'NONE',  ( -20.31707134655588121, -4.772760685475329723, 56.85231026484398598 ) ) ;
#2342 = ORIENTED_EDGE ( 'NONE', *, *, #6057, .F. ) ;
#2343 = ADVANCED_FACE ( 'NONE', ( #644 ), #8225, .T. ) ;
#2344 = ORIENTED_EDGE ( 'NONE', *, *, #11055, .T. ) ;
#2345 = CARTESIAN_POINT ( 'NONE',  ( -15.61203582817000068, -105.9033823877427096, -6.327714494218207975 ) ) ;
#2346 = LINE ( 'NONE', #1425, #9833 ) ;
#2347 = VERTEX_POINT ( 'NONE', #4084 ) ;
#2348 = DIRECTION ( 'NONE',  ( -1.000000000000000000, -1.201369187114119994E-15, -9.616040805000176517E-16 ) ) ;
#2349 = ORIENTED_EDGE ( 'NONE', *, *, #13751, .T. ) ;
#2350 = VECTOR ( 'NONE', #6228, 1000.000000000000114 ) ;
#2351 = EDGE_CURVE ( 'NONE', #10077, #9919, #10425, .T. ) ;
#2352 = DIRECTION ( 'NONE',  ( 1.000000000000000000, 1.201369187114119994E-15, 9.616040805000176517E-16 ) ) ;
#2353 = EDGE_CURVE ( 'NONE', #8123, #11256, #11047, .T. ) ;
#2354 = ITEM_DEFINED_TRANSFORMATION ( 'NONE', 'NONE', #9761,  #6789 ) ;
#2355 = CARTESIAN_POINT ( 'NONE',  ( -15.42469993581076970, -23.50709773904532085, 57.00223526491900117 ) ) ;
#2356 = DIRECTION ( 'NONE',  ( 0.5975035461963189576, 0.8018662683283437342, 0.000000000000000000 ) ) ;
#2357 = CARTESIAN_POINT ( 'NONE',  ( -23.49969986081101325, -39.82108749142274462, -10.18398123617126316 ) ) ;
#2358 = ORIENTED_EDGE ( 'NONE', *, *, #10088, .F. ) ;
#2359 = CARTESIAN_POINT ( 'NONE',  ( -10.12827607185207235, -90.53858270881919168, -5.246309576803675156 ) ) ;
#2360 = AXIS2_PLACEMENT_3D ( 'NONE', #2146, #10628, #1139 ) ;
#2361 = CARTESIAN_POINT ( 'NONE',  ( -31.79969986081099975, 20.99262100756200056, 16.16206422150100153 ) ) ;
#2362 = FACE_OUTER_BOUND ( 'NONE', #8921, .T. ) ;
#2363 = CARTESIAN_POINT ( 'NONE',  ( -8.131654986474892155, -16.81240013151894530, 56.85231026484400019 ) ) ;
#2364 = ORIENTED_EDGE ( 'NONE', *, *, #7247, .T. ) ;
#2365 = VERTEX_POINT ( 'NONE', #8817 ) ;
#2366 = DIRECTION ( 'NONE',  ( -8.018662683283439195E-16, 5.975035461963190001E-16, 1.000000000000000000 ) ) ;
#2367 = CARTESIAN_POINT ( 'NONE',  ( -20.36203582816999713, -107.1622034095870077, -6.087689735156004645 ) ) ;
#2368 = DIRECTION ( 'NONE',  ( -1.000000000000000078E-15, 1.000000000000000000, 0.000000000000000000 ) ) ;
#2369 = DIRECTION ( 'NONE',  ( -8.018662683283438208E-16, 5.975035461963189015E-16, 1.000000000000000000 ) ) ;
#2370 = AXIS2_PLACEMENT_3D ( 'NONE', #7771, #10300, #14900 ) ;
#2371 = DIRECTION ( 'NONE',  ( 1.000000000000000000, -3.922012711866029438E-32, 3.202566417187950042E-16 ) ) ;
#2372 = SHAPE_REPRESENTATION ( 'MAS-672', ( #12193, #1684, #4625, #11709, #10229, #7303, #15120, #13185, #13904, #2425, #3645, #8531, #9761 ), #2910 ) ;
#2373 = LINE ( 'NONE', #7171, #11402 ) ;
#2374 = VECTOR ( 'NONE', #4375, 1000.000000000000114 ) ;
#2375 = CARTESIAN_POINT ( 'NONE',  ( -23.09568838840838012, -16.24821979201191979, 57.00231026484397745 ) ) ;
#2376 = CARTESIAN_POINT ( 'NONE',  ( -7.707857435416944014, -48.23250629231415587, -7.308525619473091872 ) ) ;
#2377 = CARTESIAN_POINT ( 'NONE',  ( -36.19566670804134390, -37.55864118711514976, 50.77578715576750312 ) ) ;
#2378 = FACE_OUTER_BOUND ( 'NONE', #6931, .T. ) ;
#2379 = ORIENTED_EDGE ( 'NONE', *, *, #3812, .F. ) ;
#2380 = LINE ( 'NONE', #10635, #12264 ) ;
#2381 = ORIENTED_EDGE ( 'NONE', *, *, #9731, .T. ) ;
#2383 = VERTEX_POINT ( 'NONE', #7668 ) ;
#2382 = PLANE ( 'NONE',  #14009 ) ;
#2384 = EDGE_CURVE ( 'NONE', #1325, #6707, #6748, .T. ) ;
#2385 = ORIENTED_EDGE ( 'NONE', *, *, #9612, .T. ) ;
#2386 = EDGE_CURVE ( 'NONE', #10391, #3246, #2131, .T. ) ;
#2387 = DIRECTION ( 'NONE',  ( 0.9437508163134059602, 0.3306575217771102193, 5.591929034707491467E-16 ) ) ;
#2388 = VERTEX_POINT ( 'NONE', #5604 ) ;
#2389 = VECTOR ( 'NONE', #4340, 1000.000000000000000 ) ;
#2390 = DIRECTION ( 'NONE',  ( -8.018662683283438208E-16, 5.975035461963189015E-16, 1.000000000000000000 ) ) ;
#2391 = LINE ( 'NONE', #5970, #7440 ) ;
#2392 = FACE_OUTER_BOUND ( 'NONE', #5590, .T. ) ;
#2393 = VECTOR ( 'NONE', #12672, 1000.000000000000000 ) ;
#2394 = CARTESIAN_POINT ( 'NONE',  ( -15.83606446161809167, -16.37446674635458521, 51.25231026484399166 ) ) ;
#2395 = CIRCLE ( 'NONE', #5315, 0.2000000000000012046 ) ;
#2396 = CARTESIAN_POINT ( 'NONE',  ( -15.49969986081099904, -13.50737899243800122, 48.00231026484399877 ) ) ;
#2397 = DIRECTION ( 'NONE',  ( 0.000000000000000000, -1.000000000000000000, -1.224646799147350002E-16 ) ) ;
#2398 = VERTEX_POINT ( 'NONE', #2173 ) ;
#2399 = CARTESIAN_POINT ( 'NONE',  ( 5.481341784370953540, -37.42264482913269319, -11.58109560547579875 ) ) ;
#2400 = ORIENTED_EDGE ( 'NONE', *, *, #11514, .T. ) ;
#2401 = ORIENTED_EDGE ( 'NONE', *, *, #2223, .F. ) ;
#2402 = ORIENTED_EDGE ( 'NONE', *, *, #6901, .T. ) ;
#2403 = EDGE_CURVE ( 'NONE', #12952, #15056, #2324, .T. ) ;
#2404 = DIRECTION ( 'NONE',  ( -8.018662683283438208E-16, 5.975035461963189015E-16, 1.000000000000000000 ) ) ;
#2405 = VERTEX_POINT ( 'NONE', #4696 ) ;
#2406 = CARTESIAN_POINT ( 'NONE',  ( -19.27885705962587792, -22.80299515092378115, 56.81857148815599601 ) ) ;
#2407 = VECTOR ( 'NONE', #5945, 1000.000000000000114 ) ;
#2408 = VECTOR ( 'NONE', #8499, 999.9999999999998863 ) ;
#2409 = CARTESIAN_POINT ( 'NONE',  ( -13.92794721577312878, -5.586467200048621073, 57.00231026484397745 ) ) ;
#2410 = CARTESIAN_POINT ( 'NONE',  ( -11.87316907169401148, -91.00246572745722062, -9.460079019236541598 ) ) ;
#2411 = LINE ( 'NONE', #10896, #14768 ) ;
#2413 = CARTESIAN_POINT ( 'NONE',  ( -38.28773376859625444, 4.602115691098226158, 27.34154685965552645 ) ) ;
#2412 = LINE ( 'NONE', #12827, #14989 ) ;
#2414 = EDGE_LOOP ( 'NONE', ( #2044, #6800, #2303, #14872 ) ) ;
#2415 = DIRECTION ( 'NONE',  ( 8.018662683283438208E-16, -5.975035461963189015E-16, -1.000000000000000000 ) ) ;
#2416 = PLANE ( 'NONE',  #13052 ) ;
#2417 = ORIENTED_EDGE ( 'NONE', *, *, #9174, .F. ) ;
#2418 = VERTEX_POINT ( 'NONE', #2018 ) ;
#2419 = CARTESIAN_POINT ( 'NONE',  ( 21.93911714261352941, -29.45684053363936883, 26.35858622364352399 ) ) ;
#2420 = ADVANCED_FACE ( 'NONE', ( #9274 ), #11423, .F. ) ;
#2421 = DIRECTION ( 'NONE',  ( 0.9320450512859430603, -0.1645000119736390876, 0.3228494516551893012 ) ) ;
#2422 = VERTEX_POINT ( 'NONE', #1093 ) ;
#2423 = CARTESIAN_POINT ( 'NONE',  ( -13.18491133144367389, -15.23222315862922827, 51.25231026484399166 ) ) ;
#2424 = EDGE_LOOP ( 'NONE', ( #5052, #14852, #3682, #2161 ) ) ;
#2425 = AXIS2_PLACEMENT_3D ( 'NONE', #251, #4918, #9572 ) ;
#2426 = ADVANCED_FACE ( 'NONE', ( #8199 ), #3463, .T. ) ;
#2427 = LINE ( 'NONE', #7065, #969 ) ;
#2428 = VECTOR ( 'NONE', #5035, 1000.000000000000000 ) ;
#2429 = DIRECTION ( 'NONE',  ( 8.018662683283438208E-16, -5.975035461963189015E-16, -1.000000000000000000 ) ) ;
#2430 = LINE ( 'NONE', #3497, #8442 ) ;
#2431 = DIRECTION ( 'NONE',  ( 0.000000000000000000, 1.239088197126290817E-16, -1.000000000000000000 ) ) ;
#2432 = ORIENTED_EDGE ( 'NONE', *, *, #5391, .T. ) ;
#2433 = DIRECTION ( 'NONE',  ( 1.000000000000000000, 1.000000000000000078E-15, 0.000000000000000000 ) ) ;
#2434 = CARTESIAN_POINT ( 'NONE',  ( -35.74200939090608387, 6.055639158907344388, 29.62312773453597003 ) ) ;
#2435 = ORIENTED_EDGE ( 'NONE', *, *, #10473, .F. ) ;
#2436 = ADVANCED_FACE ( 'NONE', ( #6819 ), #13799, .T. ) ;
#2438 = EDGE_CURVE ( 'NONE', #5451, #7506, #13720, .T. ) ;
#2437 = CARTESIAN_POINT ( 'NONE',  ( -19.62128088291994388, -20.45131122700032833, 56.85231026484398598 ) ) ;
#2439 = ORIENTED_EDGE ( 'NONE', *, *, #6440, .F. ) ;
#2440 = DIRECTION ( 'NONE',  ( -1.000000000000000078E-15, 0.05233595624294315463, 0.9986295347545739443 ) ) ;
#2441 = EDGE_LOOP ( 'NONE', ( #7965, #7075, #10384, #1771 ) ) ;
#2442 = DIRECTION ( 'NONE',  ( -0.8543800322332384400, -0.5196486895212286683, -3.746065934159129782E-16 ) ) ;
#2443 = CARTESIAN_POINT ( 'NONE',  ( -23.02734322232803521, -10.58405290357860373, 56.85231026484398598 ) ) ;
#2444 = DIRECTION ( 'NONE',  ( 0.000000000000000000, 0.000000000000000000, -1.000000000000000000 ) ) ;
#2445 = VECTOR ( 'NONE', #14669, 1000.000000000000114 ) ;
#2446 = CARTESIAN_POINT ( 'NONE',  ( -31.79969986081099975, 20.99262100756200056, 32.26206422150099939 ) ) ;
#2447 = CARTESIAN_POINT ( 'NONE',  ( -22.13265177292497299, -18.11337496850924822, 56.85231026484398598 ) ) ;
#2448 = PLANE ( 'NONE',  #1863 ) ;
#2449 = CARTESIAN_POINT ( 'NONE',  ( -15.16333526000374832, -10.64029123852186487, 51.00231026484399166 ) ) ;
#2450 = CARTESIAN_POINT ( 'NONE',  ( -37.48126337154804588, -37.10904096101435812, 49.88474612916678552 ) ) ;
#2451 = ORIENTED_EDGE ( 'NONE', *, *, #11284, .F. ) ;
#2452 = CARTESIAN_POINT ( 'NONE',  ( -9.452813543643186378, -20.27468391147722926, 56.85231026484400019 ) ) ;
#2453 = EDGE_CURVE ( 'NONE', #4606, #2975, #5528, .T. ) ;
#2454 = EDGE_CURVE ( 'NONE', #4255, #4418, #11350, .T. ) ;
#2455 = VERTEX_POINT ( 'NONE', #6891 ) ;
#2457 = ORIENTED_EDGE ( 'NONE', *, *, #5998, .T. ) ;
#2456 = DIRECTION ( 'NONE',  ( 1.000000000000000000, 0.000000000000000000, 0.000000000000000000 ) ) ;
#2458 = ORIENTED_EDGE ( 'NONE', *, *, #669, .T. ) ;
#2459 = EDGE_CURVE ( 'NONE', #6722, #9646, #12146, .T. ) ;
#2460 = CIRCLE ( 'NONE', #8053, 9.974999999999999645 ) ;
#2461 = DIRECTION ( 'NONE',  ( 8.018662683283438208E-16, -5.975035461963189015E-16, -1.000000000000000000 ) ) ;
#2462 = ORIENTED_EDGE ( 'NONE', *, *, #12248, .T. ) ;
#2463 = CARTESIAN_POINT ( 'NONE',  ( -7.424382730750140880, -13.52981220323889566, 56.85231026484400019 ) ) ;
#2464 = DIRECTION ( 'NONE',  ( -0.8543800322332379960, -0.5196486895212294455, -3.746065934159121401E-16 ) ) ;
#2465 = LINE ( 'NONE', #7109, #8800 ) ;
#2466 = CARTESIAN_POINT ( 'NONE',  ( 18.47619366413413644, -26.09922607948998774, 8.340974680435991218 ) ) ;
#2467 = ADVANCED_FACE ( 'NONE', ( #2096 ), #950, .F. ) ;
#2468 = DIRECTION ( 'NONE',  ( 0.9183863840214728791, 0.3956847857120156520, 4.999999999999998416E-16 ) ) ;
#2469 = DIRECTION ( 'NONE',  ( -1.000000000000000000, 0.000000000000000000, 0.000000000000000000 ) ) ;
#2470 = CARTESIAN_POINT ( 'NONE',  ( 5.849866904682269997, -37.28744580235388639, -11.32700113113168250 ) ) ;
#2471 = VERTEX_POINT ( 'NONE', #6960 ) ;
#2472 = ORIENTED_EDGE ( 'NONE', *, *, #302, .F. ) ;
#2473 = ORIENTED_EDGE ( 'NONE', *, *, #13170, .T. ) ;
#2474 = CARTESIAN_POINT ( 'NONE',  ( 5.699973058922845226, -37.34275670915351952, 50.43488819123945888 ) ) ;
#2475 = ORIENTED_EDGE ( 'NONE', *, *, #6921, .T. ) ;
#2476 = VECTOR ( 'NONE', #8666, 1000.000000000000000 ) ;
#2477 = DIRECTION ( 'NONE',  ( 0.000000000000000000, -0.05233595624293968518, -0.9986295347545740553 ) ) ;
#2478 = DIRECTION ( 'NONE',  ( 0.000000000000000000, 0.000000000000000000, 1.000000000000000000 ) ) ;
#2479 = EDGE_CURVE ( 'NONE', #8450, #2196, #1020, .T. ) ;
#2480 = VECTOR ( 'NONE', #10094, 1000.000000000000000 ) ;
#2481 = DIRECTION ( 'NONE',  ( 1.000000000000000078E-15, -1.000000000000000000, 0.000000000000000000 ) ) ;
#2483 = DIRECTION ( 'NONE',  ( -1.000000000000000000, 0.000000000000000000, 0.000000000000000000 ) ) ;
#2482 = CARTESIAN_POINT ( 'NONE',  ( -7.510313973563612855, -44.09312080494210306, 20.19350477440718805 ) ) ;
#2484 = EDGE_LOOP ( 'NONE', ( #490, #90 ) ) ;
#2485 = CARTESIAN_POINT ( 'NONE',  ( -16.24681173062539230, -5.467015265965240012, 56.85231026484398598 ) ) ;
#2486 = CARTESIAN_POINT ( 'NONE',  ( -23.49969986081101325, -39.82108749142274462, -0.8113982341407446341 ) ) ;
#2487 = ORIENTED_EDGE ( 'NONE', *, *, #8691, .F. ) ;
#2488 = LINE ( 'NONE', #14197, #7615 ) ;
#2489 = ORIENTED_EDGE ( 'NONE', *, *, #1571, .T. ) ;
#2490 = SURFACE_SIDE_STYLE ('',( #1194 ) ) ;
#2491 = CIRCLE ( 'NONE', #9817, 37.50000000000000000 ) ;
#2492 = AXIS2_PLACEMENT_3D ( 'NONE', #13672, #2116, #7830 ) ;
#2493 = VECTOR ( 'NONE', #13084, 1000.000000000000114 ) ;
#2494 = DIRECTION ( 'NONE',  ( -8.018662683283438208E-16, 5.975035461963189015E-16, 1.000000000000000000 ) ) ;
#2495 = EDGE_CURVE ( 'NONE', #7103, #11225, #11159, .T. ) ;
#2496 = DIRECTION ( 'NONE',  ( -8.018662683283438208E-16, 5.975035461963189015E-16, 1.000000000000000000 ) ) ;
#2497 = CARTESIAN_POINT ( 'NONE',  ( 7.000300139189000070, -32.00737899243799944, -5.787935778498998651 ) ) ;
#2498 = DIRECTION ( 'NONE',  ( -1.000000000000000000, -1.000000000000000078E-15, 0.000000000000000000 ) ) ;
#2499 = ADVANCED_FACE ( 'NONE', ( #9191 ), #10504, .F. ) ;
#2500 = AXIS2_PLACEMENT_3D ( 'NONE', #2042, #12603, #2271 ) ;
#2501 = ORIENTED_EDGE ( 'NONE', *, *, #5983, .T. ) ;
#2502 = CARTESIAN_POINT ( 'NONE',  ( -15.49969986081099904, -19.50737899243800300, 24.21206422150100224 ) ) ;
#2503 = VECTOR ( 'NONE', #4583, 1000.000000000000114 ) ;
#2504 = DIRECTION ( 'NONE',  ( 8.018662683283438208E-16, -5.975035461963189015E-16, -1.000000000000000000 ) ) ;
#2505 = ORIENTED_EDGE ( 'NONE', *, *, #8960, .F. ) ;
#2506 = VECTOR ( 'NONE', #7833, 1000.000000000000000 ) ;
#2507 = AXIS2_PLACEMENT_3D ( 'NONE', #14562, #5302, #1864 ) ;
#2508 = DIRECTION ( 'NONE',  ( 8.018662683283438208E-16, -5.975035461963189015E-16, -1.000000000000000000 ) ) ;
#2509 = VERTEX_POINT ( 'NONE', #4848 ) ;
#2510 = CARTESIAN_POINT ( 'NONE',  ( -15.49969986081092088, -13.50737899243822504, 57.00231026484397745 ) ) ;
#2511 = EDGE_LOOP ( 'NONE', ( #13467, #8061, #11179, #554 ) ) ;
#2512 = DIRECTION ( 'NONE',  ( 1.000000000000000000, -1.291538348938060198E-32, 1.054621095516909827E-16 ) ) ;
#2513 = FACE_OUTER_BOUND ( 'NONE', #5196, .T. ) ;
#2514 = CARTESIAN_POINT ( 'NONE',  ( -15.61203582816999891, -107.9196643519486969, -5.433976602192394090 ) ) ;
#2515 = MANIFOLD_SOLID_BREP ( 'Stock-MAS-672-1', #13427 ) ;
#2516 = AXIS2_PLACEMENT_3D ( 'NONE', #2227, #9176, #7872 ) ;
#2517 = EDGE_CURVE ( 'NONE', #5816, #1460, #11877, .T. ) ;
#2518 = DIRECTION ( 'NONE',  ( -8.018662683283438208E-16, 5.975035461963189015E-16, 1.000000000000000000 ) ) ;
#2519 = EDGE_CURVE ( 'NONE', #8879, #8329, #7975, .T. ) ;
#2520 = CARTESIAN_POINT ( 'NONE',  ( -23.49969986081099904, -19.50737899243800300, 51.00231026484400587 ) ) ;
#2521 = ADVANCED_FACE ( 'NONE', ( #13116 ), #9938, .T. ) ;
#2522 = EDGE_LOOP ( 'NONE', ( #577, #10692, #12091, #12428 ) ) ;
#2523 = CARTESIAN_POINT ( 'NONE',  ( -8.994852257141582541, -49.17162665769217966, -17.42950165714590227 ) ) ;
#2524 = CARTESIAN_POINT ( 'NONE',  ( -20.79197367102019456, -108.1981419463315319, -6.432195627249867265 ) ) ;
#2525 = LINE ( 'NONE', #8483, #11808 ) ;
#2526 = ORIENTED_EDGE ( 'NONE', *, *, #12935, .F. ) ;
#2527 = FACE_OUTER_BOUND ( 'NONE', #5546, .T. ) ;
#2528 = ORIENTED_EDGE ( 'NONE', *, *, #4245, .T. ) ;
#2530 = ORIENTED_EDGE ( 'NONE', *, *, #6558, .T. ) ;
#2529 = LINE ( 'NONE', #8412, #5685 ) ;
#2531 = EDGE_CURVE ( 'NONE', #3877, #10428, #1879, .T. ) ;
#2532 = VERTEX_POINT ( 'NONE', #8097 ) ;
#2533 = AXIS2_PLACEMENT_3D ( 'NONE', #8858, #534, #13538 ) ;
#2534 = DIRECTION ( 'NONE',  ( -8.018662683283438208E-16, 5.975035461963189015E-16, 1.000000000000000000 ) ) ;
#2535 = AXIS2_PLACEMENT_3D ( 'NONE', #4631, #9204, #10362 ) ;
#2536 = VERTEX_POINT ( 'NONE', #11480 ) ;
#2537 = CYLINDRICAL_SURFACE ( 'NONE', #13422, 4.999999999999997335 ) ;
#2538 = DIRECTION ( 'NONE',  ( -0.2975196656469967227, 0.9547156899063193869, -8.090169943749448078E-16 ) ) ;
#2539 = DIRECTION ( 'NONE',  ( -0.7582332219680880669, 0.6519834208811540188, -9.975640502598240034E-16 ) ) ;
#2540 = CARTESIAN_POINT ( 'NONE',  ( 0.000000000000000000, 0.000000000000000000, 0.000000000000000000 ) ) ;
#2541 = EDGE_CURVE ( 'NONE', #5847, #7651, #1998, .T. ) ;
#2542 = LINE ( 'NONE', #14091, #2645 ) ;
#2543 = CIRCLE ( 'NONE', #6419, 6.828234652215419587 ) ;
#2544 = DIRECTION ( 'NONE',  ( 8.018662683283438208E-16, -5.975035461963189015E-16, -1.000000000000000000 ) ) ;
#2545 = DIRECTION ( 'NONE',  ( 0.8772189822852964891, -0.4800904676395362780, 9.902680687415700047E-16 ) ) ;
#2546 = EDGE_LOOP ( 'NONE', ( #8146, #2813 ) ) ;
#2547 =( BOUNDED_CURVE ( )  B_SPLINE_CURVE ( 3, ( #13910, #907, #8161, #8003 ),
 .UNSPECIFIED., .F., .T. ) 
 B_SPLINE_CURVE_WITH_KNOTS ( ( 4, 4 ),
 ( 5.266983419591660720, 5.789511490773299407 ),
 .UNSPECIFIED. ) 
 CURVE ( )  GEOMETRIC_REPRESENTATION_ITEM ( )  RATIONAL_B_SPLINE_CURVE ( ( 1.000000000000000000, 0.9773761648077839981, 0.9773761648077839981, 1.000000000000000000 ) ) 
 REPRESENTATION_ITEM ( '' )  );
#2548 = CIRCLE ( 'NONE', #11095, 6.000000000000000000 ) ;
#2549 = VERTEX_POINT ( 'NONE', #1004 ) ;
#2550 = ORIENTED_EDGE ( 'NONE', *, *, #8810, .T. ) ;
#2551 = CARTESIAN_POINT ( 'NONE',  ( -24.53816276005083452, -12.69040994830970703, 56.85231026484398598 ) ) ;
#2552 = ORIENTED_EDGE ( 'NONE', *, *, #5549, .F. ) ;
#2553 = DIRECTION ( 'NONE',  ( 0.000000000000000000, 0.000000000000000000, 1.000000000000000000 ) ) ;
#2554 = B_SPLINE_CURVE_WITH_KNOTS ( 'NONE', 3,
 ( #3175, #4403, #2028, #9978, #6676, #11361, #6954, #13733, #4096, #884, #10205, #9053, #14654, #4174, #11639, #1159, #5820, #8827, #10802, #10571, #11795, #4842, #1469, #8425, #2466, #12878, #8346, #10645 ),
 .UNSPECIFIED., .F., .F.,
 ( 4, 2, 2, 2, 2, 2, 2, 2, 2, 2, 2, 2, 2, 4 ),
 ( 0.01102632501636353554, 0.01171604659087003078, 0.01240576816537652602, 0.01309548973988301952, 0.01378521131438951476, 0.01516465446340249310, 0.01654409761241547316, 0.01792354076142845323, 0.01861326233593494500, 0.01930298391044144024, 0.01999270548494793548, 0.02068242705945443072, 0.02137214863396092943, 0.02206187020846742466 ),
 .UNSPECIFIED. ) ;
#2556 = EDGE_CURVE ( 'NONE', #818, #1516, #5737, .T. ) ;
#2555 = CARTESIAN_POINT ( 'NONE',  ( -16.28220704778704686, -23.50179128533422102, 57.00082024756494548 ) ) ;
#2557 = VECTOR ( 'NONE', #11379, 999.9999999999998863 ) ;
#2558 = DIRECTION ( 'NONE',  ( -1.000000000000000000, 0.000000000000000000, 0.000000000000000000 ) ) ;
#2559 = CARTESIAN_POINT ( 'NONE',  ( -12.42399349929057095, -91.27394999476267401, -9.904958159143182783 ) ) ;
#2560 = CARTESIAN_POINT ( 'NONE',  ( -15.49969986081099904, 22.99262100756200056, 24.21206422150099868 ) ) ;
#2561 = AXIS2_PLACEMENT_3D ( 'NONE', #11278, #11212, #5387 ) ;
#2563 = LINE ( 'NONE', #1256, #3634 ) ;
#2562 = CARTESIAN_POINT ( 'NONE',  ( -7.499699427612007696, -49.00737706678064853, -5.512197160768672610 ) ) ;
#2564 = ORIENTED_EDGE ( 'NONE', *, *, #6404, .F. ) ;
#2565 = DIRECTION ( 'NONE',  ( -3.660254037844389484E-16, 0.8386705679454246054, -0.5446390350150263071 ) ) ;
#2566 = CARTESIAN_POINT ( 'NONE',  ( -15.61203582816999713, -107.9994814593942607, -7.057848339359948042 ) ) ;
#2567 = ORIENTED_EDGE ( 'NONE', *, *, #13882, .T. ) ;
#2568 = ORIENTED_EDGE ( 'NONE', *, *, #13277, .T. ) ;
#2569 = CARTESIAN_POINT ( 'NONE',  ( 21.85920135429435263, -27.22217168940073506, 27.46206422150099868 ) ) ;
#2570 = CARTESIAN_POINT ( 'NONE',  ( -20.38418912502062952, -38.15003195939497260, 56.68542173094085257 ) ) ;
#2571 = ORIENTED_EDGE ( 'NONE', *, *, #9640, .T. ) ;
#2572 = CARTESIAN_POINT ( 'NONE',  ( -7.551842794993419261, -43.45459616270409953, -17.14591884814140954 ) ) ;
#2573 = EDGE_CURVE ( 'NONE', #1325, #8489, #10406, .T. ) ;
#2574 = EDGE_CURVE ( 'NONE', #13689, #8949, #12796, .T. ) ;
#2575 = VECTOR ( 'NONE', #863, 1000.000000000000000 ) ;
#2576 = CARTESIAN_POINT ( 'NONE',  ( -7.829332545557824652, -7.130382030772257629, 56.85231026484400019 ) ) ;
#2577 = PRODUCT_DEFINITION_SHAPE ( 'NONE', 'NONE',  #9279 ) ;
#2578 = CARTESIAN_POINT ( 'NONE',  ( -9.151507943007304746, -21.23407436738225940, 56.46085224906951083 ) ) ;
#2579 = B_SPLINE_CURVE_WITH_KNOTS ( 'NONE', 3,
 ( #1348, #10674, #206, #8820, #13434, #7372, #576, #1797, #724, #6448, #14497, #10978, #1643, #504, #12355, #9830, #8526, #6224, #6299, #2795, #5241, #13215 ),
 .UNSPECIFIED., .F., .F.,
 ( 4, 2, 2, 2, 2, 2, 2, 2, 2, 2, 4 ),
 ( 0.000000000000000000, 0.001575908489663656407, 0.002363862734495489597, 0.003151816979327322788, 0.004727725468990988736, 0.006303633958654655117, 0.007091588203486492645, 0.007879542448318330172, 0.009455450937982013901, 0.01103135942764569936, 0.01260726791730938309 ),
 .UNSPECIFIED. ) ;
#2580 = DIRECTION ( 'NONE',  ( 0.000000000000000000, 0.000000000000000000, 1.000000000000000000 ) ) ;
#2581 = LINE ( 'NONE', #1578, #14503 ) ;
#2582 = ORIENTED_EDGE ( 'NONE', *, *, #7637, .T. ) ;
#2583 = DIRECTION ( 'NONE',  ( -8.018662683283438208E-16, 5.975035461963189015E-16, 1.000000000000000000 ) ) ;
#2584 = CARTESIAN_POINT ( 'NONE',  ( -17.58300953724144122, -11.95501924286632267, 51.00231026484399166 ) ) ;
#2585 = ORIENTED_EDGE ( 'NONE', *, *, #10869, .F. ) ;
#2586 = CARTESIAN_POINT ( 'NONE',  ( -24.03943920472178775, -16.57887731378902885, 56.85231026484398598 ) ) ;
#2587 = CARTESIAN_POINT ( 'NONE',  ( -25.45346213993001427, -14.15794911993140204, 54.00231026484397745 ) ) ;
#2588 = VERTEX_POINT ( 'NONE', #1147 ) ;
#2589 = CARTESIAN_POINT ( 'NONE',  ( -13.11366204365393706, -12.47935976348540876, 51.00231026484399166 ) ) ;
#2590 = VERTEX_POINT ( 'NONE', #14850 ) ;
#2591 = ADVANCED_FACE ( 'NONE', ( #4292 ), #4446, .T. ) ;
#2592 = DIRECTION ( 'NONE',  ( -0.9437508163134049610, -0.3306575217771128283, -5.591929034707468788E-16 ) ) ;
#2593 = CARTESIAN_POINT ( 'NONE',  ( -15.49969986081099904, -27.00737899243800300, 19.50231026484400587 ) ) ;
#2594 = DIRECTION ( 'NONE',  ( 0.000000000000000000, 0.1872998510044759646, 0.9823027872370621028 ) ) ;
#2595 = PLANE ( 'NONE',  #14821 ) ;
#2596 = CIRCLE ( 'NONE', #12859, 5.000000000000000000 ) ;
#2597 = CARTESIAN_POINT ( 'NONE',  ( 15.30932787659218697, -29.23053613443893539, 2.832475549366952894 ) ) ;
#2598 = ORIENTED_EDGE ( 'NONE', *, *, #14950, .F. ) ;
#2599 = CARTESIAN_POINT ( 'NONE',  ( -15.49969986081099904, 7.183219930803499409, 5.212064221501000461 ) ) ;
#2600 = DIRECTION ( 'NONE',  ( -1.000000000000000000, -1.201369187114119994E-15, -9.616040805000176517E-16 ) ) ;
#2601 = CARTESIAN_POINT ( 'NONE',  ( -12.32172653804166096, -7.186294389320899256, 56.85231026484398598 ) ) ;
#2602 = ORIENTED_EDGE ( 'NONE', *, *, #9123, .T. ) ;
#2603 = DIRECTION ( 'NONE',  ( 0.8160499452489450301, 0.5779813897169993053, 3.090169943749371762E-16 ) ) ;
#2604 = ORIENTED_EDGE ( 'NONE', *, *, #5229, .T. ) ;
#2606 = ORIENTED_EDGE ( 'NONE', *, *, #9382, .F. ) ;
#2605 = CARTESIAN_POINT ( 'NONE',  ( -16.73644428586258570, -23.40541355628489839, 54.00231026484399166 ) ) ;
#2607 = EDGE_LOOP ( 'NONE', ( #7484, #665, #2571, #3191 ) ) ;
#2608 = EDGE_CURVE ( 'NONE', #2877, #5325, #5510, .T. ) ;
#2609 = DIRECTION ( 'NONE',  ( 0.5975035461963188466, 0.8018662683283437342, 0.000000000000000000 ) ) ;
#2610 = EDGE_LOOP ( 'NONE', ( #10492, #4620, #10315, #14610 ) ) ;
#2611 = EDGE_CURVE ( 'NONE', #7684, #5071, #5295, .T. ) ;
#2612 = CARTESIAN_POINT ( 'NONE',  ( -20.85369094651513677, -107.5158378249862352, -5.057062608101891676 ) ) ;
#2613 = DIRECTION ( 'NONE',  ( 1.000000000000000000, 0.000000000000000000, 0.000000000000000000 ) ) ;
#2614 = EDGE_CURVE ( 'NONE', #13213, #13055, #7871, .T. ) ;
#2615 = AXIS2_PLACEMENT_3D ( 'NONE', #848, #4214, #3056 ) ;
#2616 = MANIFOLD_SOLID_BREP ( 'Stock-MAS-672-1', #6319 ) ;
#2617 = FACE_OUTER_BOUND ( 'NONE', #13816, .T. ) ;
#2618 = CARTESIAN_POINT ( 'NONE',  ( -9.969334273478565933, -7.622966832294271633, 56.85231026484398598 ) ) ;
#2619 = ORIENTED_EDGE ( 'NONE', *, *, #14466, .F. ) ;
#2620 = CYLINDRICAL_SURFACE ( 'NONE', #481, 6.000000000000000000 ) ;
#2621 = ORIENTED_EDGE ( 'NONE', *, *, #9185, .F. ) ;
#2622 = AXIS2_PLACEMENT_3D ( 'NONE', #9942, #1765, #14617 ) ;
#2623 = ORIENTED_EDGE ( 'NONE', *, *, #8139, .F. ) ;
#2624 = ADVANCED_FACE ( 'NONE', ( #8390 ), #3302, .T. ) ;
#2625 = CARTESIAN_POINT ( 'NONE',  ( -23.09568838840838012, -16.24821979201191979, 56.85231026484398598 ) ) ;
#2626 = EDGE_CURVE ( 'NONE', #11664, #6233, #10994, .T. ) ;
#2627 = ORIENTED_EDGE ( 'NONE', *, *, #1777, .F. ) ;
#2628 = CARTESIAN_POINT ( 'NONE',  ( -16.91203582817000139, -107.3963282233425645, -7.315568219202335243 ) ) ;
#2629 = FACE_OUTER_BOUND ( 'NONE', #6185, .T. ) ;
#2630 = VECTOR ( 'NONE', #7244, 1000.000000000000000 ) ;
#2631 = PLANE ( 'NONE',  #12974 ) ;
#2632 = AXIS2_PLACEMENT_3D ( 'NONE', #4679, #11632, #14083 ) ;
#2633 = FACE_OUTER_BOUND ( 'NONE', #7296, .T. ) ;
#2634 =( BOUNDED_CURVE ( )  B_SPLINE_CURVE ( 3, ( #12643, #6499, #10175, #4530 ),
 .UNSPECIFIED., .F., .F. ) 
 B_SPLINE_CURVE_WITH_KNOTS ( ( 4, 4 ),
 ( 4.712388980384688786, 6.283185307179585344 ),
 .UNSPECIFIED. ) 
 CURVE ( )  GEOMETRIC_REPRESENTATION_ITEM ( )  RATIONAL_B_SPLINE_CURVE ( ( 1.000000000000000000, 0.8047378541243648264, 0.8047378541243648264, 1.000000000000000000 ) ) 
 REPRESENTATION_ITEM ( '' )  );
#2635 = CYLINDRICAL_SURFACE ( 'NONE', #2312, 6.250000000000001776 ) ;
#2637 = CARTESIAN_POINT ( 'NONE',  ( -38.47046344045732980, 4.067408198524466556, 25.52674954571450172 ) ) ;
#2636 = CARTESIAN_POINT ( 'NONE',  ( -8.667632128016617088, -19.48099602858229318, 56.85231026484400019 ) ) ;
#2638 = EDGE_LOOP ( 'NONE', ( #10828, #698, #9288, #112, #12732, #11330, #7445, #12382 ) ) ;
#2639 = CARTESIAN_POINT ( 'NONE',  ( -18.09969986081100402, -104.5552117914207741, -4.597543490852678438 ) ) ;
#2640 = VECTOR ( 'NONE', #1530, 1000.000000000000000 ) ;
#2641 = AXIS2_PLACEMENT_3D ( 'NONE', #10036, #499, #8816 ) ;
#2642 = DIRECTION ( 'NONE',  ( 8.018662683283438208E-16, -5.975035461963189015E-16, -1.000000000000000000 ) ) ;
#2643 = VERTEX_POINT ( 'NONE', #9774 ) ;
#2644 = ORIENTED_EDGE ( 'NONE', *, *, #10067, .F. ) ;
#2645 = VECTOR ( 'NONE', #11871, 1000.000000000000000 ) ;
#2646 = CARTESIAN_POINT ( 'NONE',  ( -18.08313173950247688, -36.91805501818645752, 56.91633806427406483 ) ) ;
#2647 = ADVANCED_FACE ( 'NONE', ( #10774 ), #4343, .T. ) ;
#2648 = MANIFOLD_SOLID_BREP ( 'Stock-MAS-672-1', #9007 ) ;
#2649 = EDGE_LOOP ( 'NONE', ( #3507, #9065, #989, #7814 ) ) ;
#2650 = CARTESIAN_POINT ( 'NONE',  ( 22.00030013918900096, -27.00737899243800300, 5.212064221501000461 ) ) ;
#2651 = ADVANCED_FACE ( 'NONE', ( #7541 ), #1732, .T. ) ;
#2652 = DIRECTION ( 'NONE',  ( -1.000000000000000000, -1.201369187114119994E-15, -9.616040805000176517E-16 ) ) ;
#2653 = CARTESIAN_POINT ( 'NONE',  ( -15.49969986081099904, 12.99262100756199878, 24.21206422150099868 ) ) ;
#2654 = UNCERTAINTY_MEASURE_WITH_UNIT (LENGTH_MEASURE( 1.000000000000000082E-05 ), #9849, 'distance_accuracy_value', 'NONE');
#2655 = EDGE_CURVE ( 'NONE', #10807, #13936, #12394, .T. ) ;
#2656 = CARTESIAN_POINT ( 'NONE',  ( -15.49969986081099016, -57.00737899243800655, 27.50231026484399521 ) ) ;
#2657 = CARTESIAN_POINT ( 'NONE',  ( -15.49969986081099904, -19.50737899243800300, 24.21206422150100224 ) ) ;
#2658 = VERTEX_POINT ( 'NONE', #14292 ) ;
#2659 = DIRECTION ( 'NONE',  ( 1.000000000000000000, 1.000000000000000078E-15, 0.000000000000000000 ) ) ;
#2660 = LINE ( 'NONE', #13151, #14869 ) ;
#2661 = ORIENTED_EDGE ( 'NONE', *, *, #12766, .F. ) ;
#2662 = DIRECTION ( 'NONE',  ( 0.7071067811865475727, 0.7071067811865475727, 1.202263280131018653E-17 ) ) ;
#2663 = SURFACE_STYLE_FILL_AREA ( #6088 ) ;
#2664 = ORIENTED_EDGE ( 'NONE', *, *, #10952, .F. ) ;
#2665 = CARTESIAN_POINT ( 'NONE',  ( -35.18530787408519700, 11.99262100756819827, 32.26206422150099939 ) ) ;
#2666 = ORIENTED_EDGE ( 'NONE', *, *, #5413, .T. ) ;
#2667 = VECTOR ( 'NONE', #9721, 1000.000000000000000 ) ;
#2668 = DIRECTION ( 'NONE',  ( 0.000000000000000000, 1.224646799147350002E-16, -1.000000000000000000 ) ) ;
#2669 = DIRECTION ( 'NONE',  ( -8.018662683283439195E-16, 5.975035461963190001E-16, 1.000000000000000000 ) ) ;
#2670 = DIRECTION ( 'NONE',  ( 0.5196486895212287793, -0.8543800322332385511, 9.271838545667868842E-16 ) ) ;
#2671 = LINE ( 'NONE', #1667, #4569 ) ;
#2672 = EDGE_CURVE ( 'NONE', #6427, #12430, #5036, .T. ) ;
#2673 = CARTESIAN_POINT ( 'NONE',  ( -3.508527451664998686, -47.80641709811465745, -4.747689735156000346 ) ) ;
#2674 = ORIENTED_EDGE ( 'NONE', *, *, #13007, .F. ) ;
#2675 = CARTESIAN_POINT ( 'NONE',  ( -9.539601987502633662, -5.508762965863004624, 48.00231026484398456 ) ) ;
#2676 = CARTESIAN_POINT ( 'NONE',  ( -15.61203582817000068, -107.5837463816240529, -4.877506371889844594 ) ) ;
#2677 = DIRECTION ( 'NONE',  ( 0.4491835085186243748, 0.8934395198752397294, -1.736481776669301208E-16 ) ) ;
#2678 = VERTEX_POINT ( 'NONE', #4890 ) ;
#2679 = CARTESIAN_POINT ( 'NONE',  ( -15.49969986081099904, 12.99262100756199523, 47.21206422150100224 ) ) ;
#2680 = VECTOR ( 'NONE', #8033, 1000.000000000000000 ) ;
#2681 = ORIENTED_EDGE ( 'NONE', *, *, #2574, .F. ) ;
#2683 = ORIENTED_EDGE ( 'NONE', *, *, #4717, .F. ) ;
#2682 = DIRECTION ( 'NONE',  ( -8.018662683283438208E-16, 5.975035461963189015E-16, 1.000000000000000000 ) ) ;
#2684 = ORIENTED_EDGE ( 'NONE', *, *, #11079, .F. ) ;
#2685 = AXIS2_PLACEMENT_3D ( 'NONE', #10528, #2352, #2121 ) ;
#2686 = CARTESIAN_POINT ( 'NONE',  ( -9.031792552787402784, -10.63903015472409486, 56.85231026484400019 ) ) ;
#2687 = ORIENTED_EDGE ( 'NONE', *, *, #15117, .T. ) ;
#2688 = CARTESIAN_POINT ( 'NONE',  ( -15.49969986081099371, -19.50737899243800300, -17.99768973515599768 ) ) ;
#2689 = DIRECTION ( 'NONE',  ( 0.7071067811865487940, -0.7071067811865463515, 8.659560562354927928E-17 ) ) ;
#2690 = APPLICATION_PROTOCOL_DEFINITION ( 'draft international standard', 'automotive_design', 1998, #1164 ) ;
#2691 = CARTESIAN_POINT ( 'NONE',  ( -19.40322886457036589, -11.24908093416351207, -13.08458187592522393 ) ) ;
#2692 = EDGE_CURVE ( 'NONE', #1229, #12928, #3885, .T. ) ;
#2693 = FACE_OUTER_BOUND ( 'NONE', #11328, .T. ) ;
#2694 = EDGE_CURVE ( 'NONE', #11007, #12967, #6281, .T. ) ;
#2695 = CARTESIAN_POINT ( 'NONE',  ( -20.87112600995945755, -109.7258744763782943, -5.497689735156006563 ) ) ;
#2696 = CIRCLE ( 'NONE', #12718, 19.00000000000000000 ) ;
#2697 = ORIENTED_EDGE ( 'NONE', *, *, #14813, .F. ) ;
#2698 = DIRECTION ( 'NONE',  ( 0.2640193276337003403, -0.9645173894937555392, 7.880107536067285830E-16 ) ) ;
#2699 = ORIENTED_EDGE ( 'NONE', *, *, #4522, .T. ) ;
#2700 = ORIENTED_EDGE ( 'NONE', *, *, #7662, .T. ) ;
#2701 = DIRECTION ( 'NONE',  ( -3.632077277826439854E-16, 1.000000000000000000, 0.000000000000000000 ) ) ;
#2702 = VERTEX_POINT ( 'NONE', #5478 ) ;
#2703 = ORIENTED_EDGE ( 'NONE', *, *, #10815, .F. ) ;
#2704 = DIRECTION ( 'NONE',  ( -8.018662683283438208E-16, 5.975035461963189015E-16, 1.000000000000000000 ) ) ;
#2705 = CARTESIAN_POINT ( 'NONE',  ( -12.99052370552812796, -91.62169785875414618, -10.25852757147468708 ) ) ;
#2706 = AXIS2_PLACEMENT_3D ( 'NONE', #4840, #7031, #9344 ) ;
#2707 = EDGE_CURVE ( 'NONE', #11105, #4357, #894, .T. ) ;
#2708 = EDGE_CURVE ( 'NONE', #12018, #2885, #985, .T. ) ;
#2709 = FACE_OUTER_BOUND ( 'NONE', #12674, .T. ) ;
#2711 = CARTESIAN_POINT ( 'NONE',  ( -23.02734322232803521, -10.58405290357860373, 56.85231026484398598 ) ) ;
#2710 = CARTESIAN_POINT ( 'NONE',  ( -14.61203582817000246, -106.1207381828630929, -5.933688532728891296 ) ) ;
#2712 = EDGE_CURVE ( 'NONE', #8545, #4445, #5330, .T. ) ;
#2713 = ORIENTED_EDGE ( 'NONE', *, *, #5690, .T. ) ;
#2714 = CARTESIAN_POINT ( 'NONE',  ( -23.49969986081101325, -49.19367049345325427, 14.81601876382875105 ) ) ;
#2715 = VERTEX_POINT ( 'NONE', #10756 ) ;
#2716 = CARTESIAN_POINT ( 'NONE',  ( -25.49893968439952729, -13.50738396921345519, 60.35575980305132049 ) ) ;
#2717 = ORIENTED_EDGE ( 'NONE', *, *, #9636, .T. ) ;
#2718 = ORIENTED_EDGE ( 'NONE', *, *, #11769, .F. ) ;
#2719 = LINE ( 'NONE', #14571, #778 ) ;
#2720 = ORIENTED_EDGE ( 'NONE', *, *, #6346, .F. ) ;
#2721 = ADVANCED_FACE ( 'NONE', ( #3869 ), #10433, .T. ) ;
#2722 = CARTESIAN_POINT ( 'NONE',  ( -15.49969986081099904, -57.00737899243800655, -5.497689735156002122 ) ) ;
#2723 = VECTOR ( 'NONE', #13130, 1000.000000000000000 ) ;
#2724 = LINE ( 'NONE', #7382, #8735 ) ;
#2725 = EDGE_CURVE ( 'NONE', #5304, #1083, #8572, .T. ) ;
#2726 = ADVANCED_FACE ( 'NONE', ( #7425 ), #480, .T. ) ;
#2727 = DIRECTION ( 'NONE',  ( 1.000000000000000000, 1.000000000000000078E-15, 1.000000000000000078E-15 ) ) ;
#2728 = DIRECTION ( 'NONE',  ( -0.09252159378507134047, 0.9957106782009873536, -6.691306063588577540E-16 ) ) ;
#2729 = VERTEX_POINT ( 'NONE', #547 ) ;
#2730 = CARTESIAN_POINT ( 'NONE',  ( 0.1306401100565875439, -27.07585217469818772, 58.39162460182395620 ) ) ;
#2731 = DIRECTION ( 'NONE',  ( -8.018662683283439195E-16, 5.975035461963190001E-16, 1.000000000000000000 ) ) ;
#2732 = ORIENTED_EDGE ( 'NONE', *, *, #7186, .T. ) ;
#2733 =( REPRESENTATION_RELATIONSHIP ('NONE','NONE', #2372, #410 ) REPRESENTATION_RELATIONSHIP_WITH_TRANSFORMATION ( #4647 )SHAPE_REPRESENTATION_RELATIONSHIP( ) );
#2734 = VECTOR ( 'NONE', #5531, 1000.000000000000114 ) ;
#2735 = CARTESIAN_POINT ( 'NONE',  ( -18.09969986081100402, -102.4006707610616900, -5.996718795823452020 ) ) ;
#2736 = ORIENTED_EDGE ( 'NONE', *, *, #8421, .T. ) ;
#2737 = DIRECTION ( 'NONE',  ( 0.5975035461963188466, 0.8018662683283437342, 0.000000000000000000 ) ) ;
#2738 = ORIENTED_EDGE ( 'NONE', *, *, #9988, .F. ) ;
#2739 = DIRECTION ( 'NONE',  ( 1.000000000000000078E-15, -1.000000000000000000, 0.000000000000000000 ) ) ;
#2740 = AXIS2_PLACEMENT_3D ( 'NONE', #14775, #9024, #14922 ) ;
#2741 = LINE ( 'NONE', #8320, #1351 ) ;
#2742 = ADVANCED_FACE ( 'NONE', ( #14546 ), #13478, .T. ) ;
#2743 = CARTESIAN_POINT ( 'NONE',  ( -15.61203582817000068, -106.9373417306329515, -4.908392192767062845 ) ) ;
#2744 = CARTESIAN_POINT ( 'NONE',  ( -7.844836682715777165, -47.42038978965553042, 17.17387271121222270 ) ) ;
#2745 = VECTOR ( 'NONE', #8372, 1000.000000000000000 ) ;
#2746 = VECTOR ( 'NONE', #9832, 1000.000000000000000 ) ;
#2747 = AXIS2_PLACEMENT_3D ( 'NONE', #12753, #4484, #9139 ) ;
#2748 = VECTOR ( 'NONE', #2369, 1000.000000000000000 ) ;
#2749 = DIRECTION ( 'NONE',  ( 0.000000000000000000, -1.000000000000000000, -1.224646799147350002E-16 ) ) ;
#2750 = FACE_OUTER_BOUND ( 'NONE', #13309, .T. ) ;
#2751 = ORIENTED_EDGE ( 'NONE', *, *, #6273, .T. ) ;
#2752 = CARTESIAN_POINT ( 'NONE',  ( -7.064541492512761423, -18.83173137575486322, 56.85231026484400019 ) ) ;
#2753 = CARTESIAN_POINT ( 'NONE',  ( -33.63837922572173511, -40.83713880675461638, 52.32362684487226545 ) ) ;
#2754 = VERTEX_POINT ( 'NONE', #4287 ) ;
#2755 = CARTESIAN_POINT ( 'NONE',  ( 1.891335946368680965, 9.431003388506290719, 31.86906368936717016 ) ) ;
#2756 = ORIENTED_EDGE ( 'NONE', *, *, #7653, .T. ) ;
#2758 = ORIENTED_EDGE ( 'NONE', *, *, #14490, .T. ) ;
#2757 = CARTESIAN_POINT ( 'NONE',  ( -34.27301134323082721, -39.31333522014669057, -12.96100848131858108 ) ) ;
#2759 = EDGE_LOOP ( 'NONE', ( #2926, #3220, #13340, #3548 ) ) ;
#2760 = LINE ( 'NONE', #4055, #12772 ) ;
#2761 = ORIENTED_EDGE ( 'NONE', *, *, #9743, .T. ) ;
#2762 = AXIS2_PLACEMENT_3D ( 'NONE', #2023, #6672, #879 ) ;
#2763 = EDGE_CURVE ( 'NONE', #1143, #374, #7642, .T. ) ;
#2764 = AXIS2_PLACEMENT_3D ( 'NONE', #11492, #4612, #4462 ) ;
#2765 = CARTESIAN_POINT ( 'NONE',  ( -32.80866482175071042, 10.04760564993947192, 16.37540628458954117 ) ) ;
#2766 = CARTESIAN_POINT ( 'NONE',  ( -21.21771647519868154, -9.340181373223902739, 56.85231026484398598 ) ) ;
#2767 = CARTESIAN_POINT ( 'NONE',  ( -25.46211945451987191, -14.00819915864900622, 57.00231026484397745 ) ) ;
#2768 = CARTESIAN_POINT ( 'NONE',  ( -15.21745595230144232, -22.57829892241827352, 56.85231026484400019 ) ) ;
#2769 = CIRCLE ( 'NONE', #1788, 37.50000000000000000 ) ;
#2770 = DIRECTION ( 'NONE',  ( -1.000000000000000000, -1.291538348938060198E-32, 1.054621095516909827E-16 ) ) ;
#2771 = DIRECTION ( 'NONE',  ( -8.018662683283438208E-16, 5.975035461963189015E-16, 1.000000000000000000 ) ) ;
#2772 = VECTOR ( 'NONE', #8211, 1000.000000000000000 ) ;
#2773 = ORIENTED_EDGE ( 'NONE', *, *, #11870, .F. ) ;
#2774 = CARTESIAN_POINT ( 'NONE',  ( -34.99969986081099904, -19.50737899243800300, 51.53354502093799994 ) ) ;
#2775 = ORIENTED_EDGE ( 'NONE', *, *, #4775, .F. ) ;
#2776 = ORIENTED_EDGE ( 'NONE', *, *, #5519, .F. ) ;
#2777 = CARTESIAN_POINT ( 'NONE',  ( -23.54764701038621411, -12.84694604531765272, 56.85231026484398598 ) ) ;
#2778 = EDGE_LOOP ( 'NONE', ( #7984, #14473, #2402, #2606 ) ) ;
#2779 = CARTESIAN_POINT ( 'NONE',  ( -24.41321522311770664, -15.21339595774672127, 56.85231026484398598 ) ) ;
#2780 = EDGE_CURVE ( 'NONE', #8988, #13722, #13619, .T. ) ;
#2781 = AXIS2_PLACEMENT_3D ( 'NONE', #13990, #1283, #9466 ) ;
#2782 = CYLINDRICAL_SURFACE ( 'NONE', #8299, 0.4500000000000011768 ) ;
#2783 = LINE ( 'NONE', #11035, #11210 ) ;
#2784 = VECTOR ( 'NONE', #7976, 1000.000000000000000 ) ;
#2785 = CARTESIAN_POINT ( 'NONE',  ( -38.49165779676476262, 4.011311318234620948, 23.52756386907951835 ) ) ;
#2787 = CARTESIAN_POINT ( 'NONE',  ( -36.01752465275215798, 5.923502402104435127, 18.94969861057483840 ) ) ;
#2786 = CARTESIAN_POINT ( 'NONE',  ( -7.667215781397969998, -48.40529181397006653, -7.124959850448637333 ) ) ;
#2788 = VERTEX_POINT ( 'NONE', #4139 ) ;
#2789 = CYLINDRICAL_SURFACE ( 'NONE', #8733, 4.999999999999997335 ) ;
#2790 = ORIENTED_EDGE ( 'NONE', *, *, #2178, .T. ) ;
#2791 = CARTESIAN_POINT ( 'NONE',  ( -25.45708195274498209, -14.57695636912345272, 60.36601798875501146 ) ) ;
#2792 = VERTEX_POINT ( 'NONE', #7713 ) ;
#2793 = EDGE_LOOP ( 'NONE', ( #597, #14137, #9046, #1905 ) ) ;
#2794 = AXIS2_PLACEMENT_3D ( 'NONE', #6610, #7766, #12755 ) ;
#2795 = CARTESIAN_POINT ( 'NONE',  ( -23.44796623947610570, -45.55538915506302544, 56.15044716263313518 ) ) ;
#2796 = ORIENTED_EDGE ( 'NONE', *, *, #11028, .F. ) ;
#2797 = EDGE_CURVE ( 'NONE', #7651, #13913, #11100, .T. ) ;
#2798 = VECTOR ( 'NONE', #1411, 1000.000000000000000 ) ;
#2799 = ADVANCED_FACE ( 'NONE', ( #7574 ), #13698, .F. ) ;
#2800 = CARTESIAN_POINT ( 'NONE',  ( 4.899902721674559203, 5.980169784831477209, 18.88473108487603724 ) ) ;
#2801 = CARTESIAN_POINT ( 'NONE',  ( -20.86293661740132421, -106.0955903196376227, -5.852253362411212301 ) ) ;
#2802 =( GEOMETRIC_REPRESENTATION_CONTEXT ( 3 ) GLOBAL_UNCERTAINTY_ASSIGNED_CONTEXT ( ( #10126 ) ) GLOBAL_UNIT_ASSIGNED_CONTEXT ( ( #5799, #10475, #4817 ) ) REPRESENTATION_CONTEXT ( 'NONE', 'WORKASPACE' ) );
#2803 = CARTESIAN_POINT ( 'NONE',  ( -12.47873212575276192, -23.04849409689505890, 56.88099131889190119 ) ) ;
#2804 = EDGE_CURVE ( 'NONE', #12356, #7103, #12252, .T. ) ;
#2805 = FACE_OUTER_BOUND ( 'NONE', #8180, .T. ) ;
#2806 = FACE_OUTER_BOUND ( 'NONE', #9597, .T. ) ;
#2807 = VERTEX_POINT ( 'NONE', #8794 ) ;
#2808 = PLANE ( 'NONE',  #3113 ) ;
#2809 = CARTESIAN_POINT ( 'NONE',  ( -7.495514965259227225, -43.99345095228513003, -5.653725713467976810 ) ) ;
#2810 = VERTEX_POINT ( 'NONE', #851 ) ;
#2811 = CARTESIAN_POINT ( 'NONE',  ( -7.707227416580196611, -8.855645637450560770, 57.00231026484399166 ) ) ;
#2812 = DIRECTION ( 'NONE',  ( 0.5975035461963188466, 0.8018662683283437342, 0.000000000000000000 ) ) ;
#2813 = ORIENTED_EDGE ( 'NONE', *, *, #12156, .F. ) ;
#2814 = DIRECTION ( 'NONE',  ( 0.000000000000000000, 0.000000000000000000, 1.000000000000000000 ) ) ;
#2815 = ORIENTED_EDGE ( 'NONE', *, *, #6696, .F. ) ;
#2816 = LINE ( 'NONE', #7545, #13496 ) ;
#2817 = AXIS2_PLACEMENT_3D ( 'NONE', #2314, #12875, #11713 ) ;
#2818 = EDGE_CURVE ( 'NONE', #1609, #11007, #3215, .T. ) ;
#2819 = EDGE_CURVE ( 'NONE', #8808, #11708, #11634, .T. ) ;
#2820 = FACE_BOUND ( 'NONE', #10503, .T. ) ;
#2821 = FACE_OUTER_BOUND ( 'NONE', #6571, .T. ) ;
#2822 = CARTESIAN_POINT ( 'NONE',  ( 7.000300139189000070, -32.00737899243799944, 54.21206422150100224 ) ) ;
#2823 = CARTESIAN_POINT ( 'NONE',  ( -15.42469986081099442, -23.50709773848280904, 56.85231026484400019 ) ) ;
#2824 = ORIENTED_EDGE ( 'NONE', *, *, #4138, .T. ) ;
#2825 = LINE ( 'NONE', #11308, #9943 ) ;
#2826 = CARTESIAN_POINT ( 'NONE',  ( -34.03229764406204794, -39.75996117776632843, 52.10284593195687108 ) ) ;
#2827 = VERTEX_POINT ( 'NONE', #4369 ) ;
#2828 = ORIENTED_EDGE ( 'NONE', *, *, #13827, .F. ) ;
#2830 = ORIENTED_EDGE ( 'NONE', *, *, #6730, .T. ) ;
#2829 = CARTESIAN_POINT ( 'NONE',  ( -15.49969986081099904, 0.9926210075619987805, 24.21206422150099868 ) ) ;
#2831 = VERTEX_POINT ( 'NONE', #5505 ) ;
#2832 = DIRECTION ( 'NONE',  ( -0.4274949678123838859, 0.9040177279761104634, -8.829475928589268008E-16 ) ) ;
#2833 = ORIENTED_EDGE ( 'NONE', *, *, #5507, .F. ) ;
#2834 = CARTESIAN_POINT ( 'NONE',  ( -15.49969986081091200, -13.50737899243823215, 48.00231026484398456 ) ) ;
#2835 = CIRCLE ( 'NONE', #5516, 9.974999999999999645 ) ;
#2836 = CARTESIAN_POINT ( 'NONE',  ( -7.754954776104139746, -46.50766419030464505, -2.997807438439666239 ) ) ;
#2837 = CARTESIAN_POINT ( 'NONE',  ( -20.52642601085533869, -22.12321610861327770, 57.00231026484397745 ) ) ;
#2838 = ADVANCED_FACE ( 'NONE', ( #2989 ), #4216, .F. ) ;
#2839 = DIRECTION ( 'NONE',  ( -8.018662683283438208E-16, 5.975035461963189015E-16, 1.000000000000000000 ) ) ;
#2840 = ORIENTED_EDGE ( 'NONE', *, *, #11228, .F. ) ;
#2841 = FACE_OUTER_BOUND ( 'NONE', #3843, .T. ) ;
#2842 = VERTEX_POINT ( 'NONE', #11323 ) ;
#2843 = VECTOR ( 'NONE', #12707, 1000.000000000000000 ) ;
#2844 = VERTEX_POINT ( 'NONE', #11250 ) ;
#2845 = ORIENTED_EDGE ( 'NONE', *, *, #2611, .T. ) ;
#2846 = DIRECTION ( 'NONE',  ( -1.000000000000000000, -1.201369187114119994E-15, -9.616040805000176517E-16 ) ) ;
#2847 = ORIENTED_EDGE ( 'NONE', *, *, #3607, .F. ) ;
#2848 = DIRECTION ( 'NONE',  ( 0.5975035461963189576, 0.8018662683283437342, 0.000000000000000000 ) ) ;
#2849 = CARTESIAN_POINT ( 'NONE',  ( -17.61203582817000068, -107.1622034095870077, -6.087689735156001980 ) ) ;
#2850 = CARTESIAN_POINT ( 'NONE',  ( -5.650856670168519003, -15.08880645082409444, 56.85231026484400019 ) ) ;
#2851 = VECTOR ( 'NONE', #4285, 1000.000000000000114 ) ;
#2852 = SHAPE_REPRESENTATION ( 'Boring Bar Holder', ( #6789 ), #5587 ) ;
#2853 = VECTOR ( 'NONE', #3921, 1000.000000000000000 ) ;
#2854 = PRODUCT_DEFINITION_SHAPE ( 'NONE', 'NONE',  #15126 ) ;
#2855 = EDGE_CURVE ( 'NONE', #1460, #9210, #922, .T. ) ;
#2856 = DIRECTION ( 'NONE',  ( 0.5975035461963189576, 0.8018662683283437342, 0.000000000000000000 ) ) ;
#2857 = ORIENTED_EDGE ( 'NONE', *, *, #13842, .F. ) ;
#2858 = CARTESIAN_POINT ( 'NONE',  ( -18.09969986081099336, -109.8997432187700412, -10.29035399344921764 ) ) ;
#2859 = AXIS2_PLACEMENT_3D ( 'NONE', #11837, #376, #6163 ) ;
#2860 = ORIENTED_EDGE ( 'NONE', *, *, #14251, .F. ) ;
#2861 = EDGE_CURVE ( 'NONE', #11125, #12515, #10163, .T. ) ;
#2862 = FACE_OUTER_BOUND ( 'NONE', #13166, .T. ) ;
#2863 = VERTEX_POINT ( 'NONE', #14771 ) ;
#2864 = VERTEX_POINT ( 'NONE', #14918 ) ;
#2865 = DIRECTION ( 'NONE',  ( 0.000000000000000000, 1.000000000000000000, 1.224646799147350002E-16 ) ) ;
#2866 = ORIENTED_EDGE ( 'NONE', *, *, #12920, .T. ) ;
#2867 = VECTOR ( 'NONE', #9635, 1000.000000000000000 ) ;
#2868 = CARTESIAN_POINT ( 'NONE',  ( -31.79969986081099975, 3.992621007561997892, 24.21206422150099868 ) ) ;
#2869 = FACE_OUTER_BOUND ( 'NONE', #8433, .T. ) ;
#2870 = DIRECTION ( 'NONE',  ( 0.5975035461963188466, 0.8018662683283437342, 0.000000000000000000 ) ) ;
#2871 = DIRECTION ( 'NONE',  ( -0.5401126942952660936, -0.8415927028326163351, 6.975647374412055055E-17 ) ) ;
#2872 = VECTOR ( 'NONE', #3243, 1000.000000000000114 ) ;
#2873 = DIRECTION ( 'NONE',  ( 0.000000000000000000, 1.224646799147350002E-16, -1.000000000000000000 ) ) ;
#2874 = EDGE_CURVE ( 'NONE', #6427, #6628, #13103, .T. ) ;
#2875 = FACE_BOUND ( 'NONE', #1621, .T. ) ;
#2876 = AXIS2_PLACEMENT_3D ( 'NONE', #5780, #7148, #11527 ) ;
#2877 = VERTEX_POINT ( 'NONE', #9096 ) ;
#2878 = LINE ( 'NONE', #7536, #917 ) ;
#2879 = CARTESIAN_POINT ( 'NONE',  ( -22.94870171817393256, -18.69135635822624053, 56.85231026484398598 ) ) ;
#2880 = EDGE_LOOP ( 'NONE', ( #10500, #9397, #14600, #2776 ) ) ;
#2881 = ADVANCED_FACE ( 'NONE', ( #5356 ), #10016, .F. ) ;
#2882 = CARTESIAN_POINT ( 'NONE',  ( 21.94831093474578765, -24.42285204022288880, 22.23025988852434409 ) ) ;
#2883 = ORIENTED_EDGE ( 'NONE', *, *, #6078, .T. ) ;
#2884 = DIRECTION ( 'NONE',  ( -8.018662683283438208E-16, 5.975035461963189015E-16, 1.000000000000000000 ) ) ;
#2885 = VERTEX_POINT ( 'NONE', #12398 ) ;
#2886 = DIRECTION ( 'NONE',  ( -8.018662683283438208E-16, 5.975035461963189015E-16, 1.000000000000000000 ) ) ;
#2887 = CIRCLE ( 'NONE', #8009, 10.00000000000000000 ) ;
#2888 = CARTESIAN_POINT ( 'NONE',  ( -25.26605094763165482, -15.53691377877616553, 56.85231026484398598 ) ) ;
#2889 = ADVANCED_FACE ( 'NONE', ( #770 ), #5429, .F. ) ;
#2890 = CARTESIAN_POINT ( 'NONE',  ( -7.867938255526322422, -47.21659244687067059, 17.10067396764040737 ) ) ;
#2891 = AXIS2_PLACEMENT_3D ( 'NONE', #7284, #11970, #495 ) ;
#2892 = LINE ( 'NONE', #831, #11147 ) ;
#2893 = ADVANCED_FACE ( 'NONE', ( #82 ), #998, .F. ) ;
#2894 = DIRECTION ( 'NONE',  ( -8.018662683283438208E-16, 5.975035461963189015E-16, 1.000000000000000000 ) ) ;
#2895 = ORIENTED_EDGE ( 'NONE', *, *, #979, .F. ) ;
#2896 = DIRECTION ( 'NONE',  ( 3.632077277826439854E-16, -1.000000000000000000, 0.000000000000000000 ) ) ;
#2897 = ADVANCED_FACE ( 'NONE', ( #11772 ), #3295, .T. ) ;
#2898 = CARTESIAN_POINT ( 'NONE',  ( -15.61203582817000068, -106.2504437127206529, -5.561324420954690595 ) ) ;
#2899 = LINE ( 'NONE', #8856, #13519 ) ;
#2900 = ADVANCED_FACE ( 'NONE', ( #1295 ), #7942, .T. ) ;
#2901 = VERTEX_POINT ( 'NONE', #6866 ) ;
#2902 = ORIENTED_EDGE ( 'NONE', *, *, #684, .F. ) ;
#2904 = ORIENTED_EDGE ( 'NONE', *, *, #11484, .T. ) ;
#2903 = CARTESIAN_POINT ( 'NONE',  ( -36.75660122519333584, -37.32104008884121527, -11.39096713563728258 ) ) ;
#2905 = ORIENTED_EDGE ( 'NONE', *, *, #1394, .F. ) ;
#2906 = DIRECTION ( 'NONE',  ( 0.000000000000000000, 0.000000000000000000, -1.000000000000000000 ) ) ;
#2907 = DIRECTION ( 'NONE',  ( 1.000000000000000000, 1.201369187114119994E-15, 9.616040805000176517E-16 ) ) ;
#2908 = VERTEX_POINT ( 'NONE', #2220 ) ;
#2909 = AXIS2_PLACEMENT_3D ( 'NONE', #9340, #8186, #13937 ) ;
#2910 =( GEOMETRIC_REPRESENTATION_CONTEXT ( 3 ) GLOBAL_UNCERTAINTY_ASSIGNED_CONTEXT ( ( #1145 ) ) GLOBAL_UNIT_ASSIGNED_CONTEXT ( ( #14747, #13182, #6695 ) ) REPRESENTATION_CONTEXT ( 'NONE', 'WORKASPACE' ) );
#2911 = DIRECTION ( 'NONE',  ( -8.018662683283438208E-16, 5.975035461963189015E-16, 1.000000000000000000 ) ) ;
#2912 = DIRECTION ( 'NONE',  ( -8.018662683283438208E-16, 5.975035461963189015E-16, 1.000000000000000000 ) ) ;
#2913 = LINE ( 'NONE', #3834, #1721 ) ;
#2914 = DIRECTION ( 'NONE',  ( 0.7109061395677488404, -0.7032868978765923762, 9.902680687415717796E-16 ) ) ;
#2915 = EDGE_CURVE ( 'NONE', #2185, #2996, #5952, .T. ) ;
#2916 = VECTOR ( 'NONE', #3307, 1000.000000000000114 ) ;
#2917 = CIRCLE ( 'NONE', #4141, 9.974999999999999645 ) ;
#2918 = CARTESIAN_POINT ( 'NONE',  ( -7.504222113441009867, -44.23130020225004699, 43.45950419441649615 ) ) ;
#2919 = EDGE_LOOP ( 'NONE', ( #31, #10350, #3578, #12871 ) ) ;
#2920 = EDGE_CURVE ( 'NONE', #1536, #10256, #15049, .T. ) ;
#2921 = CARTESIAN_POINT ( 'NONE',  ( -5.615565924346637594, -12.16405426399944645, 57.00231026484399166 ) ) ;
#2922 = ORIENTED_EDGE ( 'NONE', *, *, #1085, .F. ) ;
#2923 = CARTESIAN_POINT ( 'NONE',  ( -15.49969986081099194, -110.2236589786222538, -11.14993866902398700 ) ) ;
#2925 = VERTEX_POINT ( 'NONE', #3591 ) ;
#2924 = DIRECTION ( 'NONE',  ( -0.4491835085186243748, -0.8934395198752397294, 1.736481776669299976E-16 ) ) ;
#2926 = ORIENTED_EDGE ( 'NONE', *, *, #979, .T. ) ;
#2927 = DIRECTION ( 'NONE',  ( 0.08178736187250883194, 0.9966498018049948504, -5.299192642332142575E-16 ) ) ;
#2929 = VERTEX_POINT ( 'NONE', #8090 ) ;
#2928 = DIRECTION ( 'NONE',  ( 0.000000000000000000, 0.000000000000000000, 1.000000000000000000 ) ) ;
#2930 = CARTESIAN_POINT ( 'NONE',  ( -11.45455878058586663, -11.51418830146718797, -13.06929284164692540 ) ) ;
#2931 = VECTOR ( 'NONE', #12822, 1000.000000000000000 ) ;
#2932 = ADVANCED_FACE ( 'NONE', ( #12631, #10550 ), #9405, .T. ) ;
#2933 = CARTESIAN_POINT ( 'NONE',  ( -25.26605094763165482, -15.53691377877616553, 57.00231026484397745 ) ) ;
#2934 = LINE ( 'NONE', #12115, #5573 ) ;
#2935 = APPLICATION_CONTEXT ( 'automotive_design' ) ;
#2937 = DIRECTION ( 'NONE',  ( -0.2975196656470009415, 0.9547156899063180546, -8.090169943749472730E-16 ) ) ;
#2936 = CARTESIAN_POINT ( 'NONE',  ( -15.51120972694785749, -13.45872179377749589, 56.85231026484398598 ) ) ;
#2938 = VERTEX_POINT ( 'NONE', #6939 ) ;
#2939 = DIRECTION ( 'NONE',  ( -1.000000000000000000, 1.291538348938060198E-32, -1.054621095516909827E-16 ) ) ;
#2940 = CARTESIAN_POINT ( 'NONE',  ( -15.49969986081092088, -13.50737899243822504, 57.00231026484397745 ) ) ;
#2941 = VERTEX_POINT ( 'NONE', #2375 ) ;
#2942 = VERTEX_POINT ( 'NONE', #160 ) ;
#2943 = DIRECTION ( 'NONE',  ( -1.000000000000000000, 0.000000000000000000, 0.000000000000000000 ) ) ;
#2944 = ORIENTED_EDGE ( 'NONE', *, *, #9317, .F. ) ;
#2945 = CARTESIAN_POINT ( 'NONE',  ( -22.80943503306988873, -20.29474937510043020, 56.85231026484398598 ) ) ;
#2946 = VECTOR ( 'NONE', #1933, 1000.000000000000000 ) ;
#2947 = ADVANCED_FACE ( 'NONE', ( #8249 ), #2448, .T. ) ;
#2948 = CARTESIAN_POINT ( 'NONE',  ( 4.903189148188024760, 5.978594350615844988, 18.88651708455363476 ) ) ;
#2949 = CARTESIAN_POINT ( 'NONE',  ( -20.79204332525751653, -106.1260846184876385, -6.431863631274442383 ) ) ;
#2950 = DIRECTION ( 'NONE',  ( 1.000000000000000000, 0.000000000000000000, 1.224646799147350002E-16 ) ) ;
#2951 = DIRECTION ( 'NONE',  ( -1.000000000000000000, 0.000000000000000000, -1.011922027653137143E-15 ) ) ;
#2952 = ORIENTED_EDGE ( 'NONE', *, *, #5790, .T. ) ;
#2953 = FACE_OUTER_BOUND ( 'NONE', #7582, .T. ) ;
#2954 = DIRECTION ( 'NONE',  ( 1.000000000000000000, 0.000000000000000000, 0.000000000000000000 ) ) ;
#2955 = ORIENTED_EDGE ( 'NONE', *, *, #7732, .T. ) ;
#2956 = DIRECTION ( 'NONE',  ( 0.5975035461963189576, 0.8018662683283437342, 0.000000000000000000 ) ) ;
#2957 = LINE ( 'NONE', #10920, #14262 ) ;
#2958 = ORIENTED_EDGE ( 'NONE', *, *, #7054, .T. ) ;
#2959 = CARTESIAN_POINT ( 'NONE',  ( -16.34789837066772122, -3.568506607309356315, 57.00231026484397745 ) ) ;
#2960 = VECTOR ( 'NONE', #3270, 1000.000000000000000 ) ;
#2961 = EDGE_CURVE ( 'NONE', #14007, #2929, #8208, .T. ) ;
#2962 = DIRECTION ( 'NONE',  ( 0.000000000000000000, 1.000000000000000000, 1.224646799147350002E-16 ) ) ;
#2963 = EDGE_CURVE ( 'NONE', #6250, #15017, #7089, .T. ) ;
#2964 = CARTESIAN_POINT ( 'NONE',  ( -7.667215781397985097, -48.40529181396999547, 17.87504014955130316 ) ) ;
#2965 = CARTESIAN_POINT ( 'NONE',  ( -7.517426579539127296, -14.72759957212633530, 56.85231026484400019 ) ) ;
#2966 = LINE ( 'NONE', #13460, #5009 ) ;
#2967 = VERTEX_POINT ( 'NONE', #11473 ) ;
#2968 = LINE ( 'NONE', #3975, #14595 ) ;
#2969 = CARTESIAN_POINT ( 'NONE',  ( -7.754954776104139746, -46.50766419030464505, -2.997807438439666239 ) ) ;
#2970 = AXIS2_PLACEMENT_3D ( 'NONE', #9734, #11104, #2771 ) ;
#2971 = ORIENTED_EDGE ( 'NONE', *, *, #12281, .F. ) ;
#2972 = EDGE_CURVE ( 'NONE', #5899, #13245, #10324, .T. ) ;
#2974 = ORIENTED_EDGE ( 'NONE', *, *, #12809, .T. ) ;
#2973 = CARTESIAN_POINT ( 'NONE',  ( -36.26264625145540776, -37.53054613521290150, -11.72591093593669065 ) ) ;
#2975 = VERTEX_POINT ( 'NONE', #4520 ) ;
#2976 = CARTESIAN_POINT ( 'NONE',  ( -8.992083836518988349, -50.38952316532486009, 25.38445443773086296 ) ) ;
#2977 = LINE ( 'NONE', #1835, #1938 ) ;
#2978 = EDGE_CURVE ( 'NONE', #2807, #9210, #10477, .T. ) ;
#2979 = AXIS2_PLACEMENT_3D ( 'NONE', #11130, #4017, #5159 ) ;
#2980 = LINE ( 'NONE', #11391, #9083 ) ;
#2981 = EDGE_CURVE ( 'NONE', #9211, #6978, #3366, .T. ) ;
#2982 = CARTESIAN_POINT ( 'NONE',  ( -15.11203582817000246, -106.8344286703292028, -4.368659857491134169 ) ) ;
#2983 = CIRCLE ( 'NONE', #1276, 9.974999999999999645 ) ;
#2984 = TOROIDAL_SURFACE ( 'NONE', #12775, 28.00000000000000000, 5.000000000000000000 ) ;
#2985 = AXIS2_PLACEMENT_3D ( 'NONE', #1917, #7568, #14765 ) ;
#2986 = EDGE_CURVE ( 'NONE', #1083, #6348, #6, .T. ) ;
#2987 = LINE ( 'NONE', #6194, #3828 ) ;
#2988 = DIRECTION ( 'NONE',  ( -0.4800904676395363335, -0.8772189822852964891, 1.391731009600659432E-16 ) ) ;
#2989 = FACE_OUTER_BOUND ( 'NONE', #14981, .T. ) ;
#2990 = EDGE_CURVE ( 'NONE', #9086, #4893, #11393, .T. ) ;
#2991 = DIRECTION ( 'NONE',  ( -0.8018662683283438453, 0.5975035461963189576, -1.000000000000000275E-15 ) ) ;
#2992 = LINE ( 'NONE', #14401, #14463 ) ;
#2993 = AXIS2_PLACEMENT_3D ( 'NONE', #12020, #2907, #12167 ) ;
#2994 = EDGE_LOOP ( 'NONE', ( #7895, #7935, #14871, #4050 ) ) ;
#2996 = VERTEX_POINT ( 'NONE', #2520 ) ;
#2995 = CARTESIAN_POINT ( 'NONE',  ( -2.716578225681299141, -32.00737899243799944, 54.75627176226269199 ) ) ;
#2997 = ORIENTED_EDGE ( 'NONE', *, *, #3014, .T. ) ;
#2998 = CIRCLE ( 'NONE', #7875, 4.999999999999999112 ) ;
#2999 = CARTESIAN_POINT ( 'NONE',  ( -3.508527451664999575, -46.50737899243799234, -6.997689735156000346 ) ) ;
#3001 = VERTEX_POINT ( 'NONE', #4974 ) ;
#3000 = LINE ( 'NONE', #13487, #1809 ) ;
#3002 = DIRECTION ( 'NONE',  ( -0.9816271834476640867, 0.1905474982798658068, -0.009986171232787752899 ) ) ;
#3003 = EDGE_CURVE ( 'NONE', #12315, #1143, #11932, .T. ) ;
#3004 = EDGE_CURVE ( 'NONE', #13270, #2938, #14507, .T. ) ;
#3005 = FACE_OUTER_BOUND ( 'NONE', #7966, .T. ) ;
#3006 = AXIS2_PLACEMENT_3D ( 'NONE', #3820, #9639, #164 ) ;
#3007 = AXIS2_PLACEMENT_3D ( 'NONE', #4884, #5104, #12070 ) ;
#3008 = PLANE ( 'NONE',  #14727 ) ;
#3009 = ORIENTED_EDGE ( 'NONE', *, *, #10032, .T. ) ;
#3010 = DIRECTION ( 'NONE',  ( 1.000000000000000078E-15, 0.000000000000000000, -1.000000000000000000 ) ) ;
#3011 = DIRECTION ( 'NONE',  ( -8.018662683283439195E-16, 5.975035461963190001E-16, 1.000000000000000000 ) ) ;
#3012 = ORIENTED_EDGE ( 'NONE', *, *, #11136, .F. ) ;
#3013 = ORIENTED_EDGE ( 'NONE', *, *, #8586, .F. ) ;
#3014 = EDGE_CURVE ( 'NONE', #2418, #5221, #387, .T. ) ;
#3015 = CARTESIAN_POINT ( 'NONE',  ( -21.23124220554638697, -20.54376104222092181, 56.85231026484398598 ) ) ;
#3016 = ORIENTED_EDGE ( 'NONE', *, *, #4783, .F. ) ;
#3017 = LINE ( 'NONE', #7675, #2746 ) ;
#3018 = VECTOR ( 'NONE', #13674, 1000.000000000000227 ) ;
#3019 = DIRECTION ( 'NONE',  ( 0.7109061395677416240, -0.7032868978765995926, 9.902680687415702019E-16 ) ) ;
#3020 = AXIS2_PLACEMENT_3D ( 'NONE', #1127, #10309, #13834 ) ;
#3021 = DIRECTION ( 'NONE',  ( 8.659560562354914369E-17, 0.7071067811865491270, -0.7071067811865459074 ) ) ;
#3022 = CYLINDRICAL_SURFACE ( 'NONE', #4992, 8.000000000000000000 ) ;
#3023 = DIRECTION ( 'NONE',  ( 0.2975196656470014966, -0.9547156899063178326, 8.090169943749475688E-16 ) ) ;
#3024 = EDGE_LOOP ( 'NONE', ( #6929, #6851, #1300, #1195 ) ) ;
#3025 = LINE ( 'NONE', #10212, #5091 ) ;
#3026 = DIRECTION ( 'NONE',  ( -8.018662683283439195E-16, 5.975035461963190001E-16, 1.000000000000000000 ) ) ;
#3027 = EDGE_CURVE ( 'NONE', #8801, #15009, #5046, .T. ) ;
#3028 = EDGE_LOOP ( 'NONE', ( #9186, #4956, #1131, #2833 ) ) ;
#3029 = DIRECTION ( 'NONE',  ( 8.018662683283438208E-16, -5.975035461963189015E-16, -1.000000000000000000 ) ) ;
#3030 = EDGE_CURVE ( 'NONE', #6106, #1455, #1372, .T. ) ;
#3031 = LINE ( 'NONE', #7688, #5185 ) ;
#3032 = DIRECTION ( 'NONE',  ( 8.018662683283438208E-16, -5.975035461963189015E-16, -1.000000000000000000 ) ) ;
#3033 = CARTESIAN_POINT ( 'NONE',  ( -19.19431052208641475, -4.241825740657185762, 57.00231026484397745 ) ) ;
#3034 = CIRCLE ( 'NONE', #3020, 1.075000000000000400 ) ;
#3035 = ORIENTED_EDGE ( 'NONE', *, *, #8093, .T. ) ;
#3036 = CYLINDRICAL_SURFACE ( 'NONE', #4460, 8.000000000000000000 ) ;
#3037 = VECTOR ( 'NONE', #3042, 1000.000000000000114 ) ;
#3038 = DIRECTION ( 'NONE',  ( 5.000000000000000389E-16, -0.4999999999999998890, -0.8660254037844387076 ) ) ;
#3039 = SHAPE_DEFINITION_REPRESENTATION ( #542, #410 ) ;
#3040 = CARTESIAN_POINT ( 'NONE',  ( -7.654737080345058509, -48.45581950336342913, 21.06873913907410412 ) ) ;
#3041 = CARTESIAN_POINT ( 'NONE',  ( -20.44787060326519068, -4.846187890544673138, 54.00231026484397745 ) ) ;
#3042 = DIRECTION ( 'NONE',  ( 0.05771543059946734194, -0.9983330752162417054, 6.427876096865391919E-16 ) ) ;
#3043 = ORIENTED_EDGE ( 'NONE', *, *, #4422, .T. ) ;
#3044 = FACE_OUTER_BOUND ( 'NONE', #4911, .T. ) ;
#3045 = PLANE ( 'NONE',  #9471 ) ;
#3046 = AXIS2_PLACEMENT_3D ( 'NONE', #8975, #12741, #9282 ) ;
#3047 = EDGE_CURVE ( 'NONE', #8556, #14647, #6246, .T. ) ;
#3048 = ORIENTED_EDGE ( 'NONE', *, *, #181, .F. ) ;
#3050 = VERTEX_POINT ( 'NONE', #2822 ) ;
#3049 = PLANE ( 'NONE',  #2039 ) ;
#3051 = VERTEX_POINT ( 'NONE', #7242 ) ;
#3052 = CARTESIAN_POINT ( 'NONE',  ( -19.51793069539949599, -6.502732608789604463, 56.85231026484398598 ) ) ;
#3053 = LINE ( 'NONE', #2215, #6783 ) ;
#3054 = CARTESIAN_POINT ( 'NONE',  ( -100.5053766806731090, -107.1622034095863825, -7.162689735156084758 ) ) ;
#3055 = CARTESIAN_POINT ( 'NONE',  ( -8.552266936091450944, -48.47531820779182254, 46.05263013242581849 ) ) ;
#3056 = DIRECTION ( 'NONE',  ( -8.018662683283438208E-16, 5.975035461963189015E-16, 1.000000000000000000 ) ) ;
#3057 = DIRECTION ( 'NONE',  ( 1.000000000000000000, 0.000000000000000000, 0.000000000000000000 ) ) ;
#3058 = CARTESIAN_POINT ( 'NONE',  ( -38.49895354373176559, 3.992621007561999669, 23.84375914672395780 ) ) ;
#3059 = CARTESIAN_POINT ( 'NONE',  ( -7.499699860811000818, -44.42718604110348934, 43.10923419995668837 ) ) ;
#3060 = EDGE_CURVE ( 'NONE', #12888, #2455, #10704, .T. ) ;
#3061 = EDGE_LOOP ( 'NONE', ( #2262, #12581, #11511, #12338 ) ) ;
#3062 = CARTESIAN_POINT ( 'NONE',  ( -17.14283461285079824, -15.71251123034117114, 56.75231026484397745 ) ) ;
#3063 = ORIENTED_EDGE ( 'NONE', *, *, #8645, .F. ) ;
#3064 = CARTESIAN_POINT ( 'NONE',  ( -7.499699860810999041, -44.50737899243799944, -109.5506571639849938 ) ) ;
#3065 = DIRECTION ( 'NONE',  ( 0.5975035461963189576, 0.8018662683283437342, 0.000000000000000000 ) ) ;
#3067 = ORIENTED_EDGE ( 'NONE', *, *, #8714, .F. ) ;
#3066 = DIRECTION ( 'NONE',  ( -0.8018662683283436232, 0.5975035461963189576, -9.999999999999996833E-16 ) ) ;
#3068 = ORIENTED_EDGE ( 'NONE', *, *, #14490, .F. ) ;
#3069 = EDGE_CURVE ( 'NONE', #8039, #9794, #11002, .T. ) ;
#3070 = DIRECTION ( 'NONE',  ( -1.000000000000000078E-15, 1.000000000000000000, 0.000000000000000000 ) ) ;
#3072 = ORIENTED_EDGE ( 'NONE', *, *, #10681, .F. ) ;
#3071 = CARTESIAN_POINT ( 'NONE',  ( -14.61203582817000246, -106.2173407584721616, -5.758565883178084377 ) ) ;
#3073 = AXIS2_PLACEMENT_3D ( 'NONE', #1122, #15045, #2356 ) ;
#3074 = FACE_OUTER_BOUND ( 'NONE', #7797, .T. ) ;
#3075 = DIRECTION ( 'NONE',  ( -8.018662683283438208E-16, 5.975035461963189015E-16, 1.000000000000000000 ) ) ;
#3076 = CARTESIAN_POINT ( 'NONE',  ( -15.13173615696983276, -106.8354536338428034, -4.374035326349346775 ) ) ;
#3077 = DIRECTION ( 'NONE',  ( 0.000000000000000000, 1.000000000000000000, 1.224646799147350002E-16 ) ) ;
#3078 = VECTOR ( 'NONE', #525, 1000.000000000000000 ) ;
#3079 = CARTESIAN_POINT ( 'NONE',  ( -13.74242962142780478, -4.603826257390357668, 56.85231026484398598 ) ) ;
#3080 = EDGE_CURVE ( 'NONE', #11463, #5367, #310, .T. ) ;
#3081 = ORIENTED_EDGE ( 'NONE', *, *, #12175, .F. ) ;
#3082 = CARTESIAN_POINT ( 'NONE',  ( -38.49964551292070070, 3.992621007561997892, 24.26206422150100650 ) ) ;
#3083 = EDGE_CURVE ( 'NONE', #11803, #1385, #14653, .T. ) ;
#3084 = ORIENTED_EDGE ( 'NONE', *, *, #12079, .T. ) ;
#3085 = DIRECTION ( 'NONE',  ( -8.018662683283438208E-16, 5.975035461963189015E-16, 1.000000000000000000 ) ) ;
#3086 = EDGE_LOOP ( 'NONE', ( #7544, #10735, #814, #1230 ) ) ;
#3087 = ORIENTED_EDGE ( 'NONE', *, *, #102, .T. ) ;
#3088 = EDGE_CURVE ( 'NONE', #14012, #8291, #639, .T. ) ;
#3089 = CARTESIAN_POINT ( 'NONE',  ( 2.539580576486363039, -41.37673382706633873, 52.37835757418703508 ) ) ;
#3090 = VERTEX_POINT ( 'NONE', #3196 ) ;
#3091 = CARTESIAN_POINT ( 'NONE',  ( -7.794857923030186875, -46.66268402978349883, -7.997689078744453894 ) ) ;
#3092 = VECTOR ( 'NONE', #10927, 1000.000000000000227 ) ;
#3093 = DIRECTION ( 'NONE',  ( 9.263529044864487894E-17, -0.6540809579092763393, 0.7564245504347960614 ) ) ;
#3094 = CARTESIAN_POINT ( 'NONE',  ( -9.499699860810999041, -27.00737899243799234, -5.497689735155994128 ) ) ;
#3095 = AXIS2_PLACEMENT_3D ( 'NONE', #9102, #6648, #11331 ) ;
#3096 = CARTESIAN_POINT ( 'NONE',  ( -17.05536012119625866, -6.605120582739408164, 56.85231026484398598 ) ) ;
#3097 = CARTESIAN_POINT ( 'NONE',  ( -15.49969986081099904, -44.50737899243799944, -109.5506571639849938 ) ) ;
#3099 = CARTESIAN_POINT ( 'NONE',  ( 5.121633317442411126, 5.873878172623350657, 29.41645846257583941 ) ) ;
#3098 = LINE ( 'NONE', #7757, #5702 ) ;
#3100 = EDGE_LOOP ( 'NONE', ( #6231, #13537, #10368, #10274, #7595 ) ) ;
#3101 = DIRECTION ( 'NONE',  ( 0.000000000000000000, 1.000000000000000000, 1.224646799147350002E-16 ) ) ;
#3102 = EDGE_CURVE ( 'NONE', #6974, #8351, #13586, .T. ) ;
#3103 = LINE ( 'NONE', #6460, #11449 ) ;
#3104 = ORIENTED_EDGE ( 'NONE', *, *, #391, .T. ) ;
#3105 = PLANE ( 'NONE',  #8343 ) ;
#3106 = CARTESIAN_POINT ( 'NONE',  ( 21.96528430198313941, -24.18757308759200342, 22.58233337257930984 ) ) ;
#3107 = DIRECTION ( 'NONE',  ( 0.3306575217771128283, -0.9437508163134049610, 8.290375725550417844E-16 ) ) ;
#3108 = VERTEX_POINT ( 'NONE', #4269 ) ;
#3109 = AXIS2_PLACEMENT_3D ( 'NONE', #13229, #6609, #6688 ) ;
#3110 = CARTESIAN_POINT ( 'NONE',  ( -15.49969986081099904, 64.39262100756199914, 24.21206422150100579 ) ) ;
#3111 = PRODUCT_DEFINITION_SHAPE ( 'NONE', 'NONE',  #15137 ) ;
#3112 = CARTESIAN_POINT ( 'NONE',  ( -31.89126067837590028, -25.75737899243799944, -123.9247733198440073 ) ) ;
#3113 = AXIS2_PLACEMENT_3D ( 'NONE', #12442, #14433, #7612 ) ;
#3114 = DIRECTION ( 'NONE',  ( 0.000000000000000000, 0.000000000000000000, 1.000000000000000000 ) ) ;
#3115 = EDGE_CURVE ( 'NONE', #9104, #858, #7840, .T. ) ;
#3116 = CARTESIAN_POINT ( 'NONE',  ( -7.600774661673999510, -48.67202872725025031, 20.75559684966261287 ) ) ;
#3117 = CIRCLE ( 'NONE', #13865, 37.50000000000000000 ) ;
#3118 = LINE ( 'NONE', #3041, #1856 ) ;
#3119 = CARTESIAN_POINT ( 'NONE',  ( -24.28571865450477674, -8.784403367172062715, 56.85231026484398598 ) ) ;
#3120 = ORIENTED_EDGE ( 'NONE', *, *, #12366, .F. ) ;
#3121 = DIRECTION ( 'NONE',  ( 1.000000000000000000, 1.000000000000000078E-15, 0.000000000000000000 ) ) ;
#3122 =( BOUNDED_CURVE ( )  B_SPLINE_CURVE ( 3, ( #12708, #4596, #14001, #4826 ),
 .UNSPECIFIED., .F., .T. ) 
 B_SPLINE_CURVE_WITH_KNOTS ( ( 4, 4 ),
 ( 1.008260082251041245, 1.208720131788790120 ),
 .UNSPECIFIED. ) 
 CURVE ( )  GEOMETRIC_REPRESENTATION_ITEM ( )  RATIONAL_B_SPLINE_CURVE ( ( 1.000000000000000000, 0.9966541165307394312, 0.9966541165307394312, 1.000000000000000000 ) ) 
 REPRESENTATION_ITEM ( '' )  );
#3123 = DIRECTION ( 'NONE',  ( -1.169602638241520408E-15, 0.1872998510044540654, 0.9823027872370663216 ) ) ;
#3124 = ORIENTED_EDGE ( 'NONE', *, *, #12067, .F. ) ;
#3125 = VECTOR ( 'NONE', #65, 1000.000000000000114 ) ;
#3126 = VECTOR ( 'NONE', #2415, 1000.000000000000000 ) ;
#3128 = VERTEX_POINT ( 'NONE', #1900 ) ;
#3127 = DIRECTION ( 'NONE',  ( -9.702032863404950344E-16, 1.000000000000000000, 0.000000000000000000 ) ) ;
#3129 = ORIENTED_EDGE ( 'NONE', *, *, #12134, .F. ) ;
#3130 = VECTOR ( 'NONE', #5393, 1000.000000000000000 ) ;
#3131 = AXIS2_PLACEMENT_3D ( 'NONE', #3914, #12250, #1764 ) ;
#3132 = DIRECTION ( 'NONE',  ( 1.000000000000000000, 1.201369187114119994E-15, 9.616040805000176517E-16 ) ) ;
#3133 = CARTESIAN_POINT ( 'NONE',  ( -7.499699860810997265, -45.03100262877134696, 56.13904046828873362 ) ) ;
#3134 = CARTESIAN_POINT ( 'NONE',  ( -34.99969986081099904, -20.37340439622244048, -12.52892449124999885 ) ) ;
#3135 = FACE_OUTER_BOUND ( 'NONE', #9444, .T. ) ;
#3136 = EDGE_CURVE ( 'NONE', #11163, #13353, #2596, .T. ) ;
#3137 = DIRECTION ( 'NONE',  ( -1.000000000000000000, -3.700743415417187646E-16, 0.000000000000000000 ) ) ;
#3138 = CARTESIAN_POINT ( 'NONE',  ( -3.508527451664999575, -46.50737899243799234, -3.997689735156000790 ) ) ;
#3139 = CIRCLE ( 'NONE', #9383, 5.250000000000000888 ) ;
#3140 = LINE ( 'NONE', #3296, #7279 ) ;
#3141 = CARTESIAN_POINT ( 'NONE',  ( -38.49969986081099904, -37.00737899243799944, -10.11609617439569675 ) ) ;
#3142 = ORIENTED_EDGE ( 'NONE', *, *, #13101, .F. ) ;
#3143 = CARTESIAN_POINT ( 'NONE',  ( 17.56443294355201346, -29.99028402068969257, 41.90559943672241872 ) ) ;
#3144 = EDGE_LOOP ( 'NONE', ( #9522, #4695, #6183, #11406 ) ) ;
#3145 = ORIENTED_EDGE ( 'NONE', *, *, #12244, .T. ) ;
#3146 = ORIENTED_EDGE ( 'NONE', *, *, #14446, .T. ) ;
#3147 = LINE ( 'NONE', #2159, #11537 ) ;
#3148 = DIRECTION ( 'NONE',  ( 8.018662683283438208E-16, -5.975035461963189015E-16, -1.000000000000000000 ) ) ;
#3150 = ORIENTED_EDGE ( 'NONE', *, *, #10794, .F. ) ;
#3149 = FACE_OUTER_BOUND ( 'NONE', #11782, .T. ) ;
#3151 = DIRECTION ( 'NONE',  ( -8.018662683283438208E-16, 5.975035461963189015E-16, 1.000000000000000000 ) ) ;
#3152 = ADVANCED_FACE ( 'NONE', ( #14751 ), #1825, .T. ) ;
#3153 = ADVANCED_BREP_SHAPE_REPRESENTATION ( '', ( #7566, #6789 ), #8516 ) ;
#3154 = CARTESIAN_POINT ( 'NONE',  ( 7.500300139189000070, -37.00737899243799944, 19.50231026484400587 ) ) ;
#3155 =( NAMED_UNIT ( * ) PLANE_ANGLE_UNIT ( ) SI_UNIT ( $, .RADIAN. ) );
#3156 = VECTOR ( 'NONE', #7428, 1000.000000000000000 ) ;
#3157 = EDGE_CURVE ( 'NONE', #7867, #9110, #9999, .T. ) ;
#3158 = DIRECTION ( 'NONE',  ( -0.9731439732146149879, -0.2301973227387160703, -6.427876096865396850E-16 ) ) ;
#3159 = DIRECTION ( 'NONE',  ( 0.000000000000000000, 0.1872998510044759646, 0.9823027872370621028 ) ) ;
#3160 = ORIENTED_EDGE ( 'NONE', *, *, #13007, .T. ) ;
#3161 = DIRECTION ( 'NONE',  ( 1.000000000000000078E-15, -1.000000000000000000, 0.000000000000000000 ) ) ;
#3162 = VERTEX_POINT ( 'NONE', #6619 ) ;
#3163 = DIRECTION ( 'NONE',  ( -8.018662683283438208E-16, 5.975035461963189015E-16, 1.000000000000000000 ) ) ;
#3164 = ORIENTED_EDGE ( 'NONE', *, *, #2141, .T. ) ;
#3165 = VERTEX_POINT ( 'NONE', #6470 ) ;
#3166 = CARTESIAN_POINT ( 'NONE',  ( -15.49969986081099904, 2.992621007561997004, 24.21206422150099868 ) ) ;
#3167 = DIRECTION ( 'NONE',  ( 0.000000000000000000, -1.225619847157526848E-16, 1.000000000000000000 ) ) ;
#3168 = EDGE_LOOP ( 'NONE', ( #1715, #11575, #11441, #14757 ) ) ;
#3169 = B_SPLINE_CURVE_WITH_KNOTS ( 'NONE', 3,
 ( #7974, #13954, #882, #13658 ),
 .UNSPECIFIED., .F., .F.,
 ( 4, 4 ),
 ( 0.000000000000000000, 1.000000000000000000 ),
 .UNSPECIFIED. ) ;
#3170 = AXIS2_PLACEMENT_3D ( 'NONE', #10836, #10678, #10606 ) ;
#3171 = DIRECTION ( 'NONE',  ( -8.018662683283438208E-16, 5.975035461963189015E-16, 1.000000000000000000 ) ) ;
#3172 = ADVANCED_FACE ( 'NONE', ( #13531 ), #13385, .T. ) ;
#3173 = CARTESIAN_POINT ( 'NONE',  ( -28.28282149594069850, -32.00737899243799944, -15.75165123257469801 ) ) ;
#3174 = ADVANCED_FACE ( 'NONE', ( #4192 ), #4351, .F. ) ;
#3175 = CARTESIAN_POINT ( 'NONE',  ( 14.68618260102866913, -27.00737899243800300, 1.962064221501000683 ) ) ;
#3176 = EDGE_CURVE ( 'NONE', #8000, #10077, #2892, .T. ) ;
#3177 = LINE ( 'NONE', #5169, #10359 ) ;
#3179 = CARTESIAN_POINT ( 'NONE',  ( -5.898712304418588737, -10.80152183767200214, 57.00231026484399166 ) ) ;
#3178 = DIRECTION ( 'NONE',  ( 1.000000000000000000, 1.000000000000000078E-15, 0.000000000000000000 ) ) ;
#3180 = ORIENTED_EDGE ( 'NONE', *, *, #4898, .T. ) ;
#3181 = DIRECTION ( 'NONE',  ( 8.018662683283438208E-16, -5.975035461963189015E-16, -1.000000000000000000 ) ) ;
#3182 = DIRECTION ( 'NONE',  ( -0.7737441449604661736, -0.6334982226805353500, -2.419218955996689845E-16 ) ) ;
#3183 = B_SPLINE_CURVE_WITH_KNOTS ( 'NONE', 3,
 ( #6426, #1698, #5219, #11183, #14552, #5366, #12484, #14624, #702, #4067 ),
 .UNSPECIFIED., .F., .F.,
 ( 4, 2, 2, 2, 4 ),
 ( 0.2882554882889244441, 0.4355039734903317639, 0.5091282160910374222, 0.5827524586917430804, 0.8772494290945609396 ),
 .UNSPECIFIED. ) ;
#3184 = ORIENTED_EDGE ( 'NONE', *, *, #2495, .F. ) ;
#3185 = EDGE_CURVE ( 'NONE', #1753, #14533, #3118, .T. ) ;
#3186 = VERTEX_POINT ( 'NONE', #673 ) ;
#3187 = DIRECTION ( 'NONE',  ( -0.9472588896649093426, 0.3204693369899890287, -9.510565162951525763E-16 ) ) ;
#3188 = AXIS2_PLACEMENT_3D ( 'NONE', #9436, #5010, #8514 ) ;
#3189 = CARTESIAN_POINT ( 'NONE',  ( -13.18491133144367922, -15.23222315862922471, 56.75231026484399166 ) ) ;
#3190 = LINE ( 'NONE', #4563, #8642 ) ;
#3191 = ORIENTED_EDGE ( 'NONE', *, *, #11751, .F. ) ;
#3192 = CYLINDRICAL_SURFACE ( 'NONE', #8082, 8.000000000000000000 ) ;
#3193 = DIRECTION ( 'NONE',  ( 0.000000000000000000, -1.000000000000000000, -1.224646799147350002E-16 ) ) ;
#3194 = ADVANCED_FACE ( 'NONE', ( #12534 ), #12460, .F. ) ;
#3195 = CARTESIAN_POINT ( 'NONE',  ( -7.838594959942573936, -47.52544946158244699, 21.80362717976635878 ) ) ;
#3196 = CARTESIAN_POINT ( 'NONE',  ( -20.84918524500973191, -107.1622034095862972, -5.012689735156006243 ) ) ;
#3197 = CARTESIAN_POINT ( 'NONE',  ( -15.49969986081099016, -52.50737899243799944, 27.50231026484399521 ) ) ;
#3198 = ORIENTED_EDGE ( 'NONE', *, *, #13195, .F. ) ;
#3199 = CARTESIAN_POINT ( 'NONE',  ( -13.40858384722878505, -91.95517843101794142, -0.5497938619115086967 ) ) ;
#3200 = CARTESIAN_POINT ( 'NONE',  ( -19.99969986081099904, -13.50737899243800122, -13.01695671647154917 ) ) ;
#3201 = CARTESIAN_POINT ( 'NONE',  ( -19.45253106704483770, -6.466019006254929202, 57.00231026484397745 ) ) ;
#3202 = EDGE_LOOP ( 'NONE', ( #6388, #12314, #12186, #12035 ) ) ;
#3204 = ORIENTED_EDGE ( 'NONE', *, *, #3675, .F. ) ;
#3203 = CARTESIAN_POINT ( 'NONE',  ( -5.628190034013325516, -14.94052892857136250, 56.85231026484400019 ) ) ;
#3205 = VERTEX_POINT ( 'NONE', #2050 ) ;
#3206 = VECTOR ( 'NONE', #4644, 1000.000000000000000 ) ;
#3207 = ADVANCED_FACE ( 'NONE', ( #5340 ), #14673, .F. ) ;
#3208 = DIRECTION ( 'NONE',  ( 8.018662683283438208E-16, -5.975035461963189015E-16, -1.000000000000000000 ) ) ;
#3209 = DIRECTION ( 'NONE',  ( 0.9997391571607664451, 0.02283895005205794498, 7.880107536067222722E-16 ) ) ;
#3210 = CARTESIAN_POINT ( 'NONE',  ( -24.41321522311770664, -15.21339595774672127, 56.85231026484398598 ) ) ;
#3211 = CARTESIAN_POINT ( 'NONE',  ( -7.844606716089023379, -46.83718042189172337, 42.01877877715759269 ) ) ;
#3212 = CARTESIAN_POINT ( 'NONE',  ( -6.840406258826835284, -8.492485342089160838, 60.69893026050551299 ) ) ;
#3213 =( BOUNDED_CURVE ( )  B_SPLINE_CURVE ( 3, ( #2923, #6425, #11106, #5072 ),
 .UNSPECIFIED., .F., .T. ) 
 B_SPLINE_CURVE_WITH_KNOTS ( ( 4, 4 ),
 ( 0.4936738164062529632, 1.016201887587897090 ),
 .UNSPECIFIED. ) 
 CURVE ( )  GEOMETRIC_REPRESENTATION_ITEM ( )  RATIONAL_B_SPLINE_CURVE ( ( 1.000000000000000000, 0.9773761648077835540, 0.9773761648077835540, 1.000000000000000000 ) ) 
 REPRESENTATION_ITEM ( '' )  );
#3214 = AXIS2_PLACEMENT_3D ( 'NONE', #1769, #7426, #12106 ) ;
#3215 = LINE ( 'NONE', #6641, #7710 ) ;
#3216 = CARTESIAN_POINT ( 'NONE',  ( -38.49964551292070070, 3.992621007561997892, 24.16206422150099442 ) ) ;
#3217 = CARTESIAN_POINT ( 'NONE',  ( -8.858895634567669930, -20.95051974273373929, 56.85231026484400019 ) ) ;
#3218 = EDGE_LOOP ( 'NONE', ( #5826, #2203, #8296, #12869 ) ) ;
#3219 = CARTESIAN_POINT ( 'NONE',  ( 18.35491122210689596, -28.54603682261319619, 40.34048003543883709 ) ) ;
#3220 = ORIENTED_EDGE ( 'NONE', *, *, #2479, .F. ) ;
#3221 = DIRECTION ( 'NONE',  ( 0.5975035461963189576, 0.8018662683283437342, 0.000000000000000000 ) ) ;
#3223 = EDGE_LOOP ( 'NONE', ( #7297, #11784, #1458, #12605, #13746, #6701, #5995, #4937, #13540 ) ) ;
#3222 = CARTESIAN_POINT ( 'NONE',  ( -25.49893968439952729, -13.50738396921345519, 60.35575980305132049 ) ) ;
#3224 = ORIENTED_EDGE ( 'NONE', *, *, #662, .T. ) ;
#3225 = EDGE_CURVE ( 'NONE', #13665, #8073, #403, .T. ) ;
#3226 =( REPRESENTATION_RELATIONSHIP ('NONE','NONE', #2372, #10170 ) REPRESENTATION_RELATIONSHIP_WITH_TRANSFORMATION ( #14670 )SHAPE_REPRESENTATION_RELATIONSHIP( ) );
#3227 = VECTOR ( 'NONE', #15093, 1000.000000000000000 ) ;
#3228 = CARTESIAN_POINT ( 'NONE',  ( -18.09969986081100402, -109.3083623989904538, -1.510811394685556808 ) ) ;
#3229 = ORIENTED_EDGE ( 'NONE', *, *, #2692, .F. ) ;
#3230 = AXIS2_PLACEMENT_3D ( 'NONE', #6318, #2886, #3889 ) ;
#3231 = DIRECTION ( 'NONE',  ( -1.156482317317870344E-15, 1.000000000000000000, 0.000000000000000000 ) ) ;
#3232 = AXIS2_PLACEMENT_3D ( 'NONE', #1654, #3726, #7226 ) ;
#3233 = CYLINDRICAL_SURFACE ( 'NONE', #9037, 5.000000000000000000 ) ;
#3234 =( NAMED_UNIT ( * ) SI_UNIT ( $, .STERADIAN. ) SOLID_ANGLE_UNIT ( ) );
#3235 = AXIS2_PLACEMENT_3D ( 'NONE', #13228, #11223, #5400 ) ;
#3236 = VECTOR ( 'NONE', #2065, 1000.000000000000000 ) ;
#3237 = VERTEX_POINT ( 'NONE', #11080 ) ;
#3238 = CARTESIAN_POINT ( 'NONE',  ( -20.60655739512266749, -107.1622034095862972, -7.162689735156005710 ) ) ;
#3239 = AXIS2_PLACEMENT_3D ( 'NONE', #13741, #2192, #2269 ) ;
#3240 = VECTOR ( 'NONE', #9476, 1000.000000000000000 ) ;
#3241 = CARTESIAN_POINT ( 'NONE',  ( -15.49969986081091733, -13.50737899243822682, 54.00231026484399166 ) ) ;
#3242 = EDGE_LOOP ( 'NONE', ( #4773, #10389 ) ) ;
#3243 = DIRECTION ( 'NONE',  ( 0.7071067811865471286, 0.1324409947604802129, 0.6945929620337761845 ) ) ;
#3244 = ORIENTED_EDGE ( 'NONE', *, *, #3494, .T. ) ;
#3245 = CARTESIAN_POINT ( 'NONE',  ( -10.27295246487022240, -6.088325032597582620, 57.00231026484397745 ) ) ;
#3246 = VERTEX_POINT ( 'NONE', #603 ) ;
#3247 = B_SPLINE_CURVE_WITH_KNOTS ( 'NONE', 3,
 ( #11478, #12404, #11180, #11401, #1924, #5363, #10019, #4373, #929, #11254, #6795, #14848, #4444, #13556, #9100, #5656, #7947, #13628, #774, #14694, #13852, #3143, #7795, #12481, #5509, #5581, #1002, #1996, #3219, #13781, #10328, #3299, #2153, #9173 ),
 .UNSPECIFIED., .F., .F.,
 ( 4, 2, 2, 2, 2, 2, 2, 2, 2, 2, 2, 2, 2, 2, 2, 2, 4 ),
 ( 0.000000000000000000, 0.0006890873081066433998, 0.001378174616213286800, 0.002067261924319929983, 0.002756349232426573599, 0.003445436540533216782, 0.004134523848639857363, 0.004823611156746498811, 0.005512698464853139392, 0.006201785772959779973, 0.006890873081066421421, 0.007579960389173062002, 0.008269047697279702583, 0.008958135005386344898, 0.009647222313492983745, 0.01033630962159962606, 0.01102539692970626664 ),
 .UNSPECIFIED. ) ;
#3248 = ORIENTED_EDGE ( 'NONE', *, *, #650, .T. ) ;
#3249 = ADVANCED_FACE ( 'NONE', ( #5263 ), #4120, .F. ) ;
#3250 = DIRECTION ( 'NONE',  ( 1.000000000000000078E-15, 0.000000000000000000, -1.000000000000000000 ) ) ;
#3251 = ORIENTED_EDGE ( 'NONE', *, *, #4614, .T. ) ;
#3252 = DIRECTION ( 'NONE',  ( -8.018662683283438208E-16, 5.975035461963189015E-16, 1.000000000000000000 ) ) ;
#3253 = VECTOR ( 'NONE', #5654, 1000.000000000000000 ) ;
#3254 = CARTESIAN_POINT ( 'NONE',  ( -7.985436018829471294, -20.06759727486528178, 56.85231026484400019 ) ) ;
#3255 = CARTESIAN_POINT ( 'NONE',  ( -10.46773630126042498, -90.58249387939251562, -7.400451369742719443 ) ) ;
#3256 = DIRECTION ( 'NONE',  ( 0.4224988092984268695, 0.5670050759397228246, -0.7071067811865479058 ) ) ;
#3257 = CARTESIAN_POINT ( 'NONE',  ( -15.61203582816999891, -108.1070660607018397, -6.416813587133916919 ) ) ;
#3259 = FACE_OUTER_BOUND ( 'NONE', #13431, .T. ) ;
#3258 = LINE ( 'NONE', #6833, #10086 ) ;
#3260 = ORIENTED_EDGE ( 'NONE', *, *, #14867, .F. ) ;
#3261 = CARTESIAN_POINT ( 'NONE',  ( -21.12809094326923187, -9.219901432974651811, 56.85231026484398598 ) ) ;
#3262 = CARTESIAN_POINT ( 'NONE',  ( -20.87112600995945755, -110.0073789924380065, -5.497689735156006563 ) ) ;
#3263 = ORIENTED_EDGE ( 'NONE', *, *, #1396, .T. ) ;
#3264 = ORIENTED_EDGE ( 'NONE', *, *, #13201, .F. ) ;
#3265 = CARTESIAN_POINT ( 'NONE',  ( -23.59767874945767119, -17.60420555931063902, 56.85231026484398598 ) ) ;
#3266 = EDGE_CURVE ( 'NONE', #13470, #8005, #7998, .T. ) ;
#3267 = DIRECTION ( 'NONE',  ( 8.018662683283438208E-16, -5.975035461963189015E-16, -1.000000000000000000 ) ) ;
#3268 = AXIS2_PLACEMENT_3D ( 'NONE', #6836, #1041, #6908 ) ;
#3269 = ORIENTED_EDGE ( 'NONE', *, *, #9342, .T. ) ;
#3270 = DIRECTION ( 'NONE',  ( 8.018662683283438208E-16, -5.975035461963189015E-16, -1.000000000000000000 ) ) ;
#3271 = EDGE_CURVE ( 'NONE', #13499, #6704, #12610, .T. ) ;
#3272 = PLANE ( 'NONE',  #4638 ) ;
#3273 = EDGE_CURVE ( 'NONE', #14032, #7250, #1200, .T. ) ;
#3274 = VECTOR ( 'NONE', #5627, 1000.000000000000000 ) ;
#3275 = DIRECTION ( 'NONE',  ( -0.9183863840214729901, -0.3956847857120157075, -4.999999999999999402E-16 ) ) ;
#3276 = CARTESIAN_POINT ( 'NONE',  ( -31.57904533557009330, -52.92803351767890518, -14.44614973369545474 ) ) ;
#3277 = DIRECTION ( 'NONE',  ( 9.804908406240741039E-16, -0.05233595624294555548, -0.9986295347545738332 ) ) ;
#3278 = VERTEX_POINT ( 'NONE', #6922 ) ;
#3279 = CARTESIAN_POINT ( 'NONE',  ( -14.55020162889266899, -93.22838571284465559, -0.2054526157817354315 ) ) ;
#3280 = CARTESIAN_POINT ( 'NONE',  ( -21.18752042047970363, -7.775019331617081697, 56.85231026484398598 ) ) ;
#3281 = AXIS2_PLACEMENT_3D ( 'NONE', #11536, #1058, #5717 ) ;
#3282 = CARTESIAN_POINT ( 'NONE',  ( -23.54290256004220439, -7.607589560680600549, 54.00231026484397745 ) ) ;
#3283 = EDGE_CURVE ( 'NONE', #9649, #1266, #11678, .T. ) ;
#3284 = EDGE_CURVE ( 'NONE', #5304, #5925, #3325, .T. ) ;
#3285 = ORIENTED_EDGE ( 'NONE', *, *, #2861, .F. ) ;
#3286 = CARTESIAN_POINT ( 'NONE',  ( -7.307539508764906877, -16.04208977798462854, 56.85231026484400019 ) ) ;
#3287 = ORIENTED_EDGE ( 'NONE', *, *, #8298, .T. ) ;
#3288 = VECTOR ( 'NONE', #5409, 1000.000000000000114 ) ;
#3289 = DIRECTION ( 'NONE',  ( -1.000000000000000000, 0.000000000000000000, 0.000000000000000000 ) ) ;
#3290 = CARTESIAN_POINT ( 'NONE',  ( -9.472454833892761883, -49.79350169645305613, 56.51664171905113676 ) ) ;
#3291 = CARTESIAN_POINT ( 'NONE',  ( -18.48721759179251123, -17.51671033407994926, 51.00231026484399166 ) ) ;
#3292 = CARTESIAN_POINT ( 'NONE',  ( -8.872668239290053549, -48.98891758557466858, 44.15515983234535469 ) ) ;
#3293 = CARTESIAN_POINT ( 'NONE',  ( -24.85752488709640673, -10.05314452190415331, 57.00231026484397745 ) ) ;
#3294 = VECTOR ( 'NONE', #5354, 1000.000000000000000 ) ;
#3295 = CYLINDRICAL_SURFACE ( 'NONE', #12129, 0.4000000000000018541 ) ;
#3296 = CARTESIAN_POINT ( 'NONE',  ( -9.884208147447516524, -5.263176313152192698, 54.00231026484399166 ) ) ;
#3297 = CARTESIAN_POINT ( 'NONE',  ( -25.45346213993001783, -14.15794911993140026, 56.85231026484398598 ) ) ;
#3298 = ORIENTED_EDGE ( 'NONE', *, *, #12649, .T. ) ;
#3299 = CARTESIAN_POINT ( 'NONE',  ( 18.52131844622569190, -27.46537016822669841, 39.98619483191109225 ) ) ;
#3300 = EDGE_CURVE ( 'NONE', #14388, #10152, #4549, .T. ) ;
#3301 = ORIENTED_EDGE ( 'NONE', *, *, #6272, .T. ) ;
#3302 = PLANE ( 'NONE',  #10928 ) ;
#3304 = ORIENTED_EDGE ( 'NONE', *, *, #12542, .T. ) ;
#3303 = CARTESIAN_POINT ( 'NONE',  ( -23.82607259144200285, -7.937054303016555679, 60.77739987434360813 ) ) ;
#3305 = ORIENTED_EDGE ( 'NONE', *, *, #1603, .T. ) ;
#3306 = VERTEX_POINT ( 'NONE', #3344 ) ;
#3307 = DIRECTION ( 'NONE',  ( -0.9805849309054472940, -0.1960948578651647567, -6.691306063588586415E-16 ) ) ;
#3308 = CIRCLE ( 'NONE', #11851, 9.974999999999997868 ) ;
#3309 = CARTESIAN_POINT ( 'NONE',  ( -20.86505398763562269, -106.5010658813280742, -5.235401919846907504 ) ) ;
#3310 =( NAMED_UNIT ( * ) SI_UNIT ( $, .STERADIAN. ) SOLID_ANGLE_UNIT ( ) );
#3311 = EDGE_CURVE ( 'NONE', #6735, #12112, #4286, .T. ) ;
#3312 = VERTEX_POINT ( 'NONE', #14901 ) ;
#3313 = CARTESIAN_POINT ( 'NONE',  ( -21.85949554531645234, -49.38834405300886488, -17.45563142244668953 ) ) ;
#3314 = VERTEX_POINT ( 'NONE', #9151 ) ;
#3315 = CARTESIAN_POINT ( 'NONE',  ( 14.95712091018315704, -25.48139565519610983, 46.09000694556162614 ) ) ;
#3316 = ORIENTED_EDGE ( 'NONE', *, *, #8016, .T. ) ;
#3317 = CARTESIAN_POINT ( 'NONE',  ( -19.06972223273333711, -21.85101071153832919, 56.85231026484400019 ) ) ;
#3318 = ORIENTED_EDGE ( 'NONE', *, *, #15084, .T. ) ;
#3319 = ORIENTED_EDGE ( 'NONE', *, *, #5742, .T. ) ;
#3320 = CARTESIAN_POINT ( 'NONE',  ( -18.09969986081092230, -101.1019538585846931, -6.399987709240088307 ) ) ;
#3321 = ORIENTED_EDGE ( 'NONE', *, *, #2981, .T. ) ;
#3322 = DIRECTION ( 'NONE',  ( 8.018662683283438208E-16, -5.975035461963189015E-16, -1.000000000000000000 ) ) ;
#3323 = PLANE ( 'NONE',  #3046 ) ;
#3324 = CARTESIAN_POINT ( 'NONE',  ( -10.62602584962065855, -90.61080531379087688, -7.756162395898620332 ) ) ;
#3325 = CIRCLE ( 'NONE', #4060, 9.974999999999999645 ) ;
#3326 = EDGE_CURVE ( 'NONE', #11125, #2288, #12921, .T. ) ;
#3327 = CARTESIAN_POINT ( 'NONE',  ( -17.86883904694317593, -3.817807045405069655, 57.00231026484397745 ) ) ;
#3329 = CARTESIAN_POINT ( 'NONE',  ( 4.920768659932027056, 5.970170166553373292, 29.52801776241059883 ) ) ;
#3328 = CARTESIAN_POINT ( 'NONE',  ( -8.430459378593662123, -7.816413432484393020, 57.00231026484399166 ) ) ;
#3330 = EDGE_LOOP ( 'NONE', ( #10995, #14243, #7000, #3460 ) ) ;
#3331 = DIRECTION ( 'NONE',  ( 0.000000000000000000, 0.000000000000000000, -1.000000000000000000 ) ) ;
#3332 = LINE ( 'NONE', #14045, #3993 ) ;
#3333 = VERTEX_POINT ( 'NONE', #8155 ) ;
#3334 = ORIENTED_EDGE ( 'NONE', *, *, #10184, .T. ) ;
#3335 = LINE ( 'NONE', #6839, #9339 ) ;
#3336 = CARTESIAN_POINT ( 'NONE',  ( -20.78983891441731302, -38.48355218851715875, -17.62454701498858256 ) ) ;
#3337 = DIRECTION ( 'NONE',  ( 0.5975035461963188466, 0.8018662683283437342, 0.000000000000000000 ) ) ;
#3338 = ORIENTED_EDGE ( 'NONE', *, *, #3451, .F. ) ;
#3339 = DIRECTION ( 'NONE',  ( 0.9966498018049947394, -0.08178736187250883194, 8.480480961564201844E-16 ) ) ;
#3340 = DIRECTION ( 'NONE',  ( 0.000000000000000000, 1.850371707708594316E-16, -1.000000000000000000 ) ) ;
#3341 = EDGE_CURVE ( 'NONE', #11671, #855, #12844, .T. ) ;
#3342 = LINE ( 'NONE', #13753, #15071 ) ;
#3343 = VECTOR ( 'NONE', #11301, 1000.000000000000000 ) ;
#3344 = CARTESIAN_POINT ( 'NONE',  ( -15.19545581216392627, -5.437764035151672282, 57.00231026484397745 ) ) ;
#3345 = DIRECTION ( 'NONE',  ( 0.9931883319083343320, -0.1165201156931299220, 0.000000000000000000 ) ) ;
#3346 = EDGE_CURVE ( 'NONE', #4275, #1606, #13114, .T. ) ;
#3347 = ORIENTED_EDGE ( 'NONE', *, *, #8737, .T. ) ;
#3348 = CARTESIAN_POINT ( 'NONE',  ( -14.84558095633615515, -93.78297125096656828, -0.1661650273432554725 ) ) ;
#3349 = CARTESIAN_POINT ( 'NONE',  ( -3.508527451665000463, -45.20834088676133433, -4.747689735156000346 ) ) ;
#3350 = CYLINDRICAL_SURFACE ( 'NONE', #3281, 8.000000000000000000 ) ;
#3351 = VECTOR ( 'NONE', #7949, 1000.000000000000000 ) ;
#3352 = DIRECTION ( 'NONE',  ( 0.000000000000000000, 1.000000000000000000, 1.224646799147350002E-16 ) ) ;
#3353 = ORIENTED_EDGE ( 'NONE', *, *, #10501, .T. ) ;
#3354 = DIRECTION ( 'NONE',  ( 0.000000000000000000, 0.000000000000000000, 1.000000000000000000 ) ) ;
#3355 = ORIENTED_EDGE ( 'NONE', *, *, #1777, .T. ) ;
#3356 = PLANE ( 'NONE',  #10321 ) ;
#3357 = CARTESIAN_POINT ( 'NONE',  ( 0.8003001391889992266, 20.99262100756200056, 32.26206422150099939 ) ) ;
#3358 = VECTOR ( 'NONE', #9461, 1000.000000000000000 ) ;
#3359 = EDGE_CURVE ( 'NONE', #6669, #413, #13905, .T. ) ;
#3360 = AXIS2_PLACEMENT_3D ( 'NONE', #6803, #10260, #1008 ) ;
#3361 = CARTESIAN_POINT ( 'NONE',  ( -5.923714809816990723, -16.30043024566306187, 56.85231026484400019 ) ) ;
#3362 = CARTESIAN_POINT ( 'NONE',  ( -9.539601987502633662, -5.508762965863004624, 48.00231026484398456 ) ) ;
#3363 = ADVANCED_FACE ( 'NONE', ( #5558 ), #13826, .T. ) ;
#3364 = CARTESIAN_POINT ( 'NONE',  ( -5.586161854270613958, -12.19953394658199386, 60.37797296075051889 ) ) ;
#3365 = EDGE_CURVE ( 'NONE', #6540, #10777, #2107, .T. ) ;
#3366 = LINE ( 'NONE', #7012, #2843 ) ;
#3367 = EDGE_CURVE ( 'NONE', #4531, #9738, #6771, .T. ) ;
#3368 = VECTOR ( 'NONE', #313, 1000.000000000000000 ) ;
#3369 = VECTOR ( 'NONE', #11512, 1000.000000000000000 ) ;
#3370 = CARTESIAN_POINT ( 'NONE',  ( 13.85920135429429934, -27.00737899243800300, 27.46206422150099868 ) ) ;
#3371 = CARTESIAN_POINT ( 'NONE',  ( -15.61203582817000068, -106.9748017008338365, -5.104852750214476487 ) ) ;
#3372 = AXIS2_PLACEMENT_3D ( 'NONE', #6454, #13511, #7752 ) ;
#3373 = ORIENTED_EDGE ( 'NONE', *, *, #7991, .F. ) ;
#3374 = LINE ( 'NONE', #8255, #11281 ) ;
#3375 = VERTEX_POINT ( 'NONE', #9303 ) ;
#3377 = ORIENTED_EDGE ( 'NONE', *, *, #568, .T. ) ;
#3376 = DIRECTION ( 'NONE',  ( 0.9805849309054470719, 0.1960948578651654506, 6.691306063588581484E-16 ) ) ;
#3378 = ADVANCED_FACE ( 'NONE', ( #10382 ), #11455, .F. ) ;
#3379 = VERTEX_POINT ( 'NONE', #8232 ) ;
#3380 = CARTESIAN_POINT ( 'NONE',  ( -30.62513859619093637, -27.95036676736707548, 53.90694524323490100 ) ) ;
#3381 = ORIENTED_EDGE ( 'NONE', *, *, #7456, .T. ) ;
#3382 = CARTESIAN_POINT ( 'NONE',  ( -37.04494295528539993, 0.9926210075619987805, 32.26206422150099939 ) ) ;
#3383 = VECTOR ( 'NONE', #2368, 1000.000000000000000 ) ;
#3384 = CARTESIAN_POINT ( 'NONE',  ( -20.84918524500973902, -106.9855902083963173, -5.012689735156002691 ) ) ;
#3385 = EDGE_CURVE ( 'NONE', #9045, #8329, #2430, .T. ) ;
#3386 = EDGE_CURVE ( 'NONE', #11066, #5017, #12616, .T. ) ;
#3387 = EDGE_CURVE ( 'NONE', #8000, #1003, #2835, .T. ) ;
#3388 = EDGE_LOOP ( 'NONE', ( #12923, #11052, #857, #12832 ) ) ;
#3389 = CIRCLE ( 'NONE', #3882, 1.249999999999999778 ) ;
#3390 = CARTESIAN_POINT ( 'NONE',  ( -2.216578225681298697, -32.00737899243799944, -10.85656391856669778 ) ) ;
#3391 = ORIENTED_EDGE ( 'NONE', *, *, #14678, .T. ) ;
#3392 = CARTESIAN_POINT ( 'NONE',  ( -10.99969986081099904, -13.50737899243800122, -13.01695671647155983 ) ) ;
#3393 = EDGE_LOOP ( 'NONE', ( #5436, #8272, #6501 ) ) ;
#3394 = EDGE_LOOP ( 'NONE', ( #11502, #10470, #13969, #14163 ) ) ;
#3395 = ORIENTED_EDGE ( 'NONE', *, *, #6434, .T. ) ;
#3396 = DIRECTION ( 'NONE',  ( -8.018662683283438208E-16, 5.975035461963189015E-16, 1.000000000000000000 ) ) ;
#3397 = CARTESIAN_POINT ( 'NONE',  ( -18.09969986081100046, -107.1622034095870077, -6.087689735156001980 ) ) ;
#3398 = ORIENTED_EDGE ( 'NONE', *, *, #9222, .T. ) ;
#3400 = ADVANCED_FACE ( 'NONE', ( #439 ), #1354, .F. ) ;
#3399 = CARTESIAN_POINT ( 'NONE',  ( -21.63983770886135005, -21.40953461391054802, 56.49919483392252317 ) ) ;
#3401 = AXIS2_PLACEMENT_3D ( 'NONE', #1059, #12777, #5718 ) ;
#3402 = CARTESIAN_POINT ( 'NONE',  ( -24.21370508435883906, -8.652820519829269585, 56.85231026484398598 ) ) ;
#3403 = DIRECTION ( 'NONE',  ( 0.000000000000000000, 0.000000000000000000, 1.000000000000000000 ) ) ;
#3405 = CARTESIAN_POINT ( 'NONE',  ( 3.107080982810261460, 6.836425395121002779, 30.39410943549851751 ) ) ;
#3404 = CARTESIAN_POINT ( 'NONE',  ( -15.51120972694785749, -13.45872179377749589, 56.85231026484398598 ) ) ;
#3406 = VERTEX_POINT ( 'NONE', #371 ) ;
#3407 = CARTESIAN_POINT ( 'NONE',  ( -5.596483669297567687, -12.31283553816471610, 54.00231026484399166 ) ) ;
#3408 = CIRCLE ( 'NONE', #13917, 9.974999999999999645 ) ;
#3409 = CARTESIAN_POINT ( 'NONE',  ( -13.88982576282654691, -4.575998618238553917, 56.85231026484398598 ) ) ;
#3410 = EDGE_LOOP ( 'NONE', ( #7448, #14536, #13432, #9681 ) ) ;
#3411 = VECTOR ( 'NONE', #14729, 1000.000000000000000 ) ;
#3412 = ORIENTED_EDGE ( 'NONE', *, *, #11526, .T. ) ;
#3413 = PLANE ( 'NONE',  #792 ) ;
#3414 = LINE ( 'NONE', #1967, #1273 ) ;
#3415 = DIRECTION ( 'NONE',  ( -0.9999272109403024578, 0.01206535623791937274, -8.090169943749475688E-16 ) ) ;
#3416 = VERTEX_POINT ( 'NONE', #6005 ) ;
#3417 = CARTESIAN_POINT ( 'NONE',  ( -15.61203582816999891, -107.8822043817477976, -5.237516044744981336 ) ) ;
#3418 = ADVANCED_FACE ( 'NONE', ( #9687 ), #9611, .T. ) ;
#3419 = CARTESIAN_POINT ( 'NONE',  ( 22.00030013918900096, -27.00737899243800300, 2.712064221501000461 ) ) ;
#3420 = LINE ( 'NONE', #8070, #1899 ) ;
#3421 = CARTESIAN_POINT ( 'NONE',  ( -16.32407967933980686, -20.53418644068968746, 56.85231026484400019 ) ) ;
#3422 = CARTESIAN_POINT ( 'NONE',  ( -15.49969986081099371, -18.00737899243799944, -13.28793577849899776 ) ) ;
#3424 = VERTEX_POINT ( 'NONE', #2656 ) ;
#3423 = VECTOR ( 'NONE', #14036, 1000.000000000000000 ) ;
#3425 = CARTESIAN_POINT ( 'NONE',  ( 22.00030013918900096, -27.00737899243800300, 5.212064221501000461 ) ) ;
#3426 = CARTESIAN_POINT ( 'NONE',  ( -5.499699860810998153, -46.50737899243799944, -5.497689735156003010 ) ) ;
#3427 = PLANE ( 'NONE',  #9129 ) ;
#3428 = CARTESIAN_POINT ( 'NONE',  ( -20.48903913017556633, -19.85700446605285308, 56.85231026484398598 ) ) ;
#3429 = VERTEX_POINT ( 'NONE', #9458 ) ;
#3430 = ORIENTED_EDGE ( 'NONE', *, *, #282, .T. ) ;
#3431 = EDGE_CURVE ( 'NONE', #13608, #13647, #1271, .T. ) ;
#3432 = CARTESIAN_POINT ( 'NONE',  ( -15.45378054160984682, -13.48759475315262613, 56.85231026484398598 ) ) ;
#3433 = CARTESIAN_POINT ( 'NONE',  ( -8.703838785437527648, -17.86878899887247130, 56.85231026484400019 ) ) ;
#3434 = EDGE_CURVE ( 'NONE', #7373, #12214, #4095, .T. ) ;
#3435 = AXIS2_PLACEMENT_3D ( 'NONE', #10644, #1389, #14089 ) ;
#3436 = LINE ( 'NONE', #2446, #11771 ) ;
#3437 = CARTESIAN_POINT ( 'NONE',  ( -9.376966593418606166, -18.77214511605354019, 56.85231026484400019 ) ) ;
#3438 = CARTESIAN_POINT ( 'NONE',  ( -17.81448839017816610, -11.78253482624722537, 51.25231026484399166 ) ) ;
#3439 = DIRECTION ( 'NONE',  ( -1.000000000000000000, -3.632077277826439854E-16, 0.000000000000000000 ) ) ;
#3440 = CARTESIAN_POINT ( 'NONE',  ( -20.82328182105635150, -108.2441250888176256, -6.239265671067229846 ) ) ;
#3441 = PLANE ( 'NONE',  #6165 ) ;
#3442 = ORIENTED_EDGE ( 'NONE', *, *, #10501, .F. ) ;
#3443 = DIRECTION ( 'NONE',  ( 1.000000000000000000, 1.201369187114119994E-15, 9.616040805000176517E-16 ) ) ;
#3444 = PRODUCT_DEFINITION_CONTEXT ( 'detailed design', #13204, 'design' ) ;
#3445 = ORIENTED_EDGE ( 'NONE', *, *, #3900, .T. ) ;
#3447 = VERTEX_POINT ( 'NONE', #2497 ) ;
#3446 = CARTESIAN_POINT ( 'NONE',  ( -20.51036999038052144, -4.847632558696703953, 61.37692998373628228 ) ) ;
#3448 = ORIENTED_EDGE ( 'NONE', *, *, #3014, .F. ) ;
#3449 = ADVANCED_FACE ( 'NONE', ( #10683 ), #8303, .F. ) ;
#3450 = CYLINDRICAL_SURFACE ( 'NONE', #14121, 22.99999999999999645 ) ;
#3451 = EDGE_CURVE ( 'NONE', #9434, #11163, #5028, .T. ) ;
#3452 = VERTEX_POINT ( 'NONE', #289 ) ;
#3453 = EDGE_CURVE ( 'NONE', #1539, #8623, #14072, .T. ) ;
#3454 = CARTESIAN_POINT ( 'NONE',  ( -23.52886110248590867, -17.73748770914800943, 57.00231026484397745 ) ) ;
#3455 = AXIS2_PLACEMENT_3D ( 'NONE', #10736, #3339, #2197 ) ;
#3456 = DIRECTION ( 'NONE',  ( -8.018662683283438208E-16, 5.975035461963189015E-16, 1.000000000000000000 ) ) ;
#3457 = EDGE_CURVE ( 'NONE', #2729, #2060, #7700, .T. ) ;
#3458 = CARTESIAN_POINT ( 'NONE',  ( -20.45368390747784204, -7.130130991507916072, 56.85231026484398598 ) ) ;
#3459 = VECTOR ( 'NONE', #631, 1000.000000000000114 ) ;
#3460 = ORIENTED_EDGE ( 'NONE', *, *, #9073, .F. ) ;
#3461 = CARTESIAN_POINT ( 'NONE',  ( 6.268676098693725329, -37.15669500878450293, -11.03356574139771418 ) ) ;
#3462 = ORIENTED_EDGE ( 'NONE', *, *, #980, .T. ) ;
#3463 = PLANE ( 'NONE',  #8955 ) ;
#3464 = ORIENTED_EDGE ( 'NONE', *, *, #15043, .F. ) ;
#3465 = ORIENTED_EDGE ( 'NONE', *, *, #3284, .F. ) ;
#3466 = VECTOR ( 'NONE', #3902, 1000.000000000000227 ) ;
#3467 = ADVANCED_FACE ( 'NONE', ( #7384 ), #13146, .F. ) ;
#3468 = FACE_OUTER_BOUND ( 'NONE', #13387, .T. ) ;
#3469 = EDGE_CURVE ( 'NONE', #3791, #2288, #7307, .T. ) ;
#3470 = VERTEX_POINT ( 'NONE', #11990 ) ;
#3471 = PLANE ( 'NONE',  #7869 ) ;
#3472 = LINE ( 'NONE', #1178, #3784 ) ;
#3473 = CIRCLE ( 'NONE', #13978, 3.000000000000002665 ) ;
#3474 = CARTESIAN_POINT ( 'NONE',  ( -22.42051587769119791, -8.443926053929422082, 57.00231026484397745 ) ) ;
#3475 = AXIS2_PLACEMENT_3D ( 'NONE', #2367, #14144, #4737 ) ;
#3476 = VECTOR ( 'NONE', #4225, 1000.000000000000000 ) ;
#3477 = CARTESIAN_POINT ( 'NONE',  ( -7.508989031724891738, -44.91746444383585413, 21.43160362669583563 ) ) ;
#3479 = DIRECTION ( 'NONE',  ( -8.018662683283438208E-16, 5.975035461963189015E-16, 1.000000000000000000 ) ) ;
#3478 = CARTESIAN_POINT ( 'NONE',  ( -15.49969986081092088, -13.50737899243822504, 57.00231026484397745 ) ) ;
#3480 = ORIENTED_EDGE ( 'NONE', *, *, #10083, .F. ) ;
#3481 = LINE ( 'NONE', #3407, #2393 ) ;
#3482 = CYLINDRICAL_SURFACE ( 'NONE', #10342, 8.000000000000000000 ) ;
#3483 = ORIENTED_EDGE ( 'NONE', *, *, #10090, .T. ) ;
#3484 = EDGE_LOOP ( 'NONE', ( #8028, #12864, #10850, #4126 ) ) ;
#3485 = CARTESIAN_POINT ( 'NONE',  ( -18.15085299098534577, -14.64962258016358199, 56.75231026484397745 ) ) ;
#3486 = CARTESIAN_POINT ( 'NONE',  ( -23.49969986081099904, -43.98440953699977740, -17.13441993860073609 ) ) ;
#3487 = ORIENTED_EDGE ( 'NONE', *, *, #6004, .F. ) ;
#3488 = VECTOR ( 'NONE', #3171, 1000.000000000000000 ) ;
#3489 = CARTESIAN_POINT ( 'NONE',  ( -8.559440489995196799, -40.49367064263154248, -17.35106608438774956 ) ) ;
#3490 = VERTEX_POINT ( 'NONE', #1577 ) ;
#3491 = VECTOR ( 'NONE', #12558, 999.9999999999998863 ) ;
#3492 = CARTESIAN_POINT ( 'NONE',  ( -20.59651154950486784, -18.41489981358536809, 56.85231026484398598 ) ) ;
#3493 = CARTESIAN_POINT ( 'NONE',  ( 9.000300139189000959, -19.50737899243799589, -4.178074911655800250 ) ) ;
#3494 = EDGE_CURVE ( 'NONE', #2060, #775, #1506, .T. ) ;
#3495 = ADVANCED_FACE ( 'NONE', ( #2805, #7457 ), #5931, .T. ) ;
#3496 = AXIS2_PLACEMENT_3D ( 'NONE', #10402, #15068, #5876 ) ;
#3497 = CARTESIAN_POINT ( 'NONE',  ( -5.499699860810999041, -19.50737899243799589, 6.712064221500998684 ) ) ;
#3498 = CARTESIAN_POINT ( 'NONE',  ( -21.79367780933653265, -21.24601366423100401, 54.00231026484399166 ) ) ;
#3499 = ORIENTED_EDGE ( 'NONE', *, *, #5632, .F. ) ;
#3500 = VECTOR ( 'NONE', #2728, 1000.000000000000114 ) ;
#3501 = CARTESIAN_POINT ( 'NONE',  ( -11.11913394994981807, -90.72833461817117495, -2.380443756164408509 ) ) ;
#3502 = CARTESIAN_POINT ( 'NONE',  ( -35.87823185118522673, 5.990273379230379724, 29.55080429321562363 ) ) ;
#3503 = CARTESIAN_POINT ( 'NONE',  ( -15.49969986081100082, -107.0696085497772430, -4.320874558545138022 ) ) ;
#3504 = LINE ( 'NONE', #4655, #3892 ) ;
#3505 = EDGE_LOOP ( 'NONE', ( #426, #15038 ) ) ;
#3506 = CARTESIAN_POINT ( 'NONE',  ( -15.45180655762527699, -13.52173975529984418, 56.85231026484398598 ) ) ;
#3507 = ORIENTED_EDGE ( 'NONE', *, *, #9532, .T. ) ;
#3508 = CARTESIAN_POINT ( 'NONE',  ( -7.887638505697304403, -19.95386229157006497, 54.00231026484400587 ) ) ;
#3509 = DIRECTION ( 'NONE',  ( 1.000000000000000078E-15, -1.000000000000000000, 0.000000000000000000 ) ) ;
#3510 = CIRCLE ( 'NONE', #6673, 0.2000000000000012046 ) ;
#3511 = FACE_OUTER_BOUND ( 'NONE', #3410, .T. ) ;
#3512 = DIRECTION ( 'NONE',  ( 1.000000000000000000, 1.000000000000000078E-15, 0.000000000000000000 ) ) ;
#3513 = CARTESIAN_POINT ( 'NONE',  ( -5.500158185064795369, -14.04218574468902148, 60.35427179981845569 ) ) ;
#3514 = AXIS2_PLACEMENT_3D ( 'NONE', #8054, #12826, #9131 ) ;
#3515 = EDGE_CURVE ( 'NONE', #7319, #6946, #8643, .T. ) ;
#3516 = CARTESIAN_POINT ( 'NONE',  ( -9.425865349984700714, -18.82901260770113794, 56.85231026484400019 ) ) ;
#3517 = CARTESIAN_POINT ( 'NONE',  ( -7.836123178633707553, -47.48973556348613556, -7.797900083227910173 ) ) ;
#3518 = DIRECTION ( 'NONE',  ( -0.8415927028326188886, 0.5401126942952620968, -9.975640502598240034E-16 ) ) ;
#3519 = CIRCLE ( 'NONE', #10104, 0.2000000000000012046 ) ;
#3520 = DIRECTION ( 'NONE',  ( -0.9731439732146150989, -0.2301973227387161258, -6.427876096865397836E-16 ) ) ;
#3521 = VERTEX_POINT ( 'NONE', #7564 ) ;
#3522 = DIRECTION ( 'NONE',  ( -8.018662683283438208E-16, 5.975035461963189015E-16, 1.000000000000000000 ) ) ;
#3523 = ORIENTED_EDGE ( 'NONE', *, *, #14196, .F. ) ;
#3525 = ORIENTED_EDGE ( 'NONE', *, *, #593, .T. ) ;
#3524 = CARTESIAN_POINT ( 'NONE',  ( -25.40982920130948841, -12.19918686643515038, 60.37889978234523625 ) ) ;
#3526 = VERTEX_POINT ( 'NONE', #5131 ) ;
#3527 = DIRECTION ( 'NONE',  ( -0.9040177279761056894, -0.4274949678123940444, -4.694715627858810513E-16 ) ) ;
#3528 = VERTEX_POINT ( 'NONE', #9720 ) ;
#3529 = CIRCLE ( 'NONE', #6690, 0.1499999999999989397 ) ;
#3530 = FACE_OUTER_BOUND ( 'NONE', #12405, .T. ) ;
#3531 = DIRECTION ( 'NONE',  ( 0.000000000000000000, 0.000000000000000000, -1.000000000000000000 ) ) ;
#3532 = CONICAL_SURFACE ( 'NONE', #4519, 1.750000000000000666, 0.2709468503384208082 ) ;
#3533 = CARTESIAN_POINT ( 'NONE',  ( -1.425463962227826897, -54.93314309385483085, -15.32525311590548434 ) ) ;
#3534 = DIRECTION ( 'NONE',  ( 1.000000000000000000, 0.000000000000000000, 0.000000000000000000 ) ) ;
#3535 = DIRECTION ( 'NONE',  ( -0.8934395198752397294, 0.4491835085186243748, -9.848077530122081084E-16 ) ) ;
#3536 = EDGE_CURVE ( 'NONE', #11027, #1495, #14965, .T. ) ;
#3537 = CARTESIAN_POINT ( 'NONE',  ( -3.508527451664999575, -46.50737899243799234, -6.997689735156000346 ) ) ;
#3538 = CARTESIAN_POINT ( 'NONE',  ( -15.49969986081086226, -13.50737899243826767, -13.99768973515600301 ) ) ;
#3539 = EDGE_CURVE ( 'NONE', #9881, #10505, #2983, .T. ) ;
#3540 = ORIENTED_EDGE ( 'NONE', *, *, #8696, .T. ) ;
#3541 = CARTESIAN_POINT ( 'NONE',  ( 5.815276763445654140, -37.29975643136119601, -11.35092641676986780 ) ) ;
#3542 = VERTEX_POINT ( 'NONE', #12242 ) ;
#3543 = DIRECTION ( 'NONE',  ( 0.000000000000000000, 1.000000000000000000, 1.224646799147350002E-16 ) ) ;
#3544 = ORIENTED_EDGE ( 'NONE', *, *, #1222, .F. ) ;
#3545 = ORIENTED_EDGE ( 'NONE', *, *, #9387, .F. ) ;
#3546 = CARTESIAN_POINT ( 'NONE',  ( 0.8003001391889992266, 11.99262100756199878, 16.16206422150100153 ) ) ;
#3547 = DIRECTION ( 'NONE',  ( -8.018662683283439195E-16, 5.975035461963190001E-16, 1.000000000000000000 ) ) ;
#3548 = ORIENTED_EDGE ( 'NONE', *, *, #12653, .T. ) ;
#3549 = CARTESIAN_POINT ( 'NONE',  ( -20.04324321135802833, -22.41562731333683089, 56.72605870807743145 ) ) ;
#3550 = ADVANCED_FACE ( 'NONE', ( #321 ), #6109, .F. ) ;
#3551 = DIRECTION ( 'NONE',  ( 0.000000000000000000, 9.130123557772668334E-17, -1.000000000000000000 ) ) ;
#3552 = CARTESIAN_POINT ( 'NONE',  ( -11.88635259617872819, -91.00826541128077452, -9.472131609326678969 ) ) ;
#3553 = ADVANCED_FACE ( 'NONE', ( #11013 ), #400, .F. ) ;
#3554 = ADVANCED_FACE ( 'NONE', ( #614 ), #5059, .T. ) ;
#3555 = DIRECTION ( 'NONE',  ( 0.000000000000000000, -0.1872998510044983078, -0.9823027872370578839 ) ) ;
#3557 = FACE_OUTER_BOUND ( 'NONE', #12087, .T. ) ;
#3556 = CARTESIAN_POINT ( 'NONE',  ( -5.628190034013325516, -14.94052892857136250, 57.00231026484399166 ) ) ;
#3558 = ORIENTED_EDGE ( 'NONE', *, *, #9996, .F. ) ;
#3559 = DIRECTION ( 'NONE',  ( 0.1165201156931293391, 0.9931883319083343320, -4.999999999999998416E-16 ) ) ;
#3560 = DIRECTION ( 'NONE',  ( -0.8160499452489514693, -0.5779813897169900905, -3.090169943749478258E-16 ) ) ;
#3561 = ORIENTED_EDGE ( 'NONE', *, *, #3469, .F. ) ;
#3562 = EDGE_LOOP ( 'NONE', ( #6332, #6855, #7002, #1600 ) ) ;
#3563 = CARTESIAN_POINT ( 'NONE',  ( 21.92071449028411934, -29.15732165064080661, 26.65852393176527713 ) ) ;
#3564 = LINE ( 'NONE', #6144, #11293 ) ;
#3565 = EDGE_LOOP ( 'NONE', ( #6068, #8853, #12260, #14273 ) ) ;
#3566 = CARTESIAN_POINT ( 'NONE',  ( -11.49146427699059814, -37.56416174903810656, -17.78544053839978289 ) ) ;
#3567 = VERTEX_POINT ( 'NONE', #4130 ) ;
#3568 = VECTOR ( 'NONE', #1054, 1000.000000000000000 ) ;
#3569 = FACE_OUTER_BOUND ( 'NONE', #11700, .T. ) ;
#3570 = CONTEXT_DEPENDENT_SHAPE_REPRESENTATION ( #11530, #3111 ) ;
#3571 = EDGE_CURVE ( 'NONE', #7124, #186, #7257, .T. ) ;
#3572 = DIRECTION ( 'NONE',  ( -1.000000000000000000, 3.922012711866029438E-32, -3.202566417187950042E-16 ) ) ;
#3573 = DIRECTION ( 'NONE',  ( 0.9085715390340232123, -0.4177292884839972631, 9.781476007338056784E-16 ) ) ;
#3574 = ORIENTED_EDGE ( 'NONE', *, *, #3607, .T. ) ;
#3575 = DIRECTION ( 'NONE',  ( 8.018662683283438208E-16, -5.975035461963189015E-16, -1.000000000000000000 ) ) ;
#3576 = VECTOR ( 'NONE', #3439, 1000.000000000000000 ) ;
#3577 = CARTESIAN_POINT ( 'NONE',  ( -35.90258886980872433, 5.978594350616473818, 29.53761135844903052 ) ) ;
#3578 = ORIENTED_EDGE ( 'NONE', *, *, #3451, .T. ) ;
#3579 = CARTESIAN_POINT ( 'NONE',  ( -15.49969986081092088, -13.50737899243822504, 57.00231026484397745 ) ) ;
#3580 = EDGE_LOOP ( 'NONE', ( #7576, #346, #4068, #6028 ) ) ;
#3581 = CARTESIAN_POINT ( 'NONE',  ( -22.70913108387521007, -17.14542124616560770, 56.85231026484398598 ) ) ;
#3582 = EDGE_LOOP ( 'NONE', ( #14028, #2505, #15092, #11861, #4506 ) ) ;
#3583 = LINE ( 'NONE', #6859, #11295 ) ;
#3584 = DIRECTION ( 'NONE',  ( 0.000000000000000000, 0.000000000000000000, -1.000000000000000000 ) ) ;
#3585 = CARTESIAN_POINT ( 'NONE',  ( -17.71337442941458207, -109.6899368550501919, -1.875748381208218740 ) ) ;
#3586 = ADVANCED_FACE ( 'NONE', ( #14609 ), #10795, .T. ) ;
#3587 = DIRECTION ( 'NONE',  ( 0.7032868978765922652, 0.7109061395677488404, 1.391731009600549485E-16 ) ) ;
#3588 = AXIS2_PLACEMENT_3D ( 'NONE', #1990, #6863, #11550 ) ;
#3589 = LINE ( 'NONE', #12939, #608 ) ;
#3590 = DIRECTION ( 'NONE',  ( -8.018662683283438208E-16, 5.975035461963189015E-16, 1.000000000000000000 ) ) ;
#3591 = CARTESIAN_POINT ( 'NONE',  ( -24.80452494096261873, -9.912819877918101596, 57.00231026484397745 ) ) ;
#3592 = LINE ( 'NONE', #5802, #3947 ) ;
#3593 = CIRCLE ( 'NONE', #12929, 9.974999999999999645 ) ;
#3594 = CARTESIAN_POINT ( 'NONE',  ( -3.499699860810999041, -57.00737899243800655, -16.02584758213710003 ) ) ;
#3595 = CARTESIAN_POINT ( 'NONE',  ( -11.68798435751175369, -21.74340199640734994, 56.85231026484400019 ) ) ;
#3596 = EDGE_LOOP ( 'NONE', ( #10331, #1203, #8201, #6576, #5146, #9852 ) ) ;
#3597 = CARTESIAN_POINT ( 'NONE',  ( -14.61203582817000068, -107.1622034095870077, -6.087689735155999315 ) ) ;
#3598 = ORIENTED_EDGE ( 'NONE', *, *, #12152, .F. ) ;
#3599 = VECTOR ( 'NONE', #12995, 1000.000000000000000 ) ;
#3601 = ORIENTED_EDGE ( 'NONE', *, *, #8217, .T. ) ;
#3600 = CARTESIAN_POINT ( 'NONE',  ( -23.42445533997705454, -9.084766574938008432, 56.85231026484398598 ) ) ;
#3602 = VERTEX_POINT ( 'NONE', #3982 ) ;
#3603 = DIRECTION ( 'NONE',  ( 1.000000000000000000, 1.201369187114119994E-15, 9.616040805000176517E-16 ) ) ;
#3604 = ORIENTED_EDGE ( 'NONE', *, *, #1207, .F. ) ;
#3605 = AXIS2_PLACEMENT_3D ( 'NONE', #7315, #10849, #1586 ) ;
#3606 = CARTESIAN_POINT ( 'NONE',  ( -12.84854673063649599, -12.36513540471286809, 51.00231026484399166 ) ) ;
#3607 = EDGE_CURVE ( 'NONE', #8564, #150, #3827, .T. ) ;
#3608 = DIRECTION ( 'NONE',  ( 0.000000000000000000, 9.130123557772668334E-17, -1.000000000000000000 ) ) ;
#3609 = CARTESIAN_POINT ( 'NONE',  ( -24.05607732349520234, -14.07716379046991584, 56.85231026484398598 ) ) ;
#3610 =( LENGTH_UNIT ( ) NAMED_UNIT ( * ) SI_UNIT ( .MILLI., .METRE. ) );
#3611 = CIRCLE ( 'NONE', #11429, 9.974999999999999645 ) ;
#3612 = CARTESIAN_POINT ( 'NONE',  ( -19.54288648179596422, -11.51027871586804352, -13.06950530299294577 ) ) ;
#3613 = VECTOR ( 'NONE', #14283, 1000.000000000000114 ) ;
#3614 = CARTESIAN_POINT ( 'NONE',  ( -7.499699860810998153, -44.50737899243799944, 56.13904046828873362 ) ) ;
#3615 = CARTESIAN_POINT ( 'NONE',  ( -21.12809094326923187, -9.219901432974651811, 57.00231026484397745 ) ) ;
#3616 = DIRECTION ( 'NONE',  ( -8.018662683283439195E-16, 5.975035461963190001E-16, 1.000000000000000000 ) ) ;
#3617 = ORIENTED_EDGE ( 'NONE', *, *, #1798, .F. ) ;
#3618 = ORIENTED_EDGE ( 'NONE', *, *, #4318, .F. ) ;
#3619 = VERTEX_POINT ( 'NONE', #13178 ) ;
#3620 = CARTESIAN_POINT ( 'NONE',  ( 2.818822887961262236, -40.24903322726662225, 52.22360476062456769 ) ) ;
#3621 = EDGE_LOOP ( 'NONE', ( #9381, #14454, #10489 ) ) ;
#3622 = CIRCLE ( 'NONE', #5566, 3.000000000000002665 ) ;
#3623 = CARTESIAN_POINT ( 'NONE',  ( -21.45979773411919922, -21.50599501901345789, 48.00231026484398456 ) ) ;
#3624 = EDGE_CURVE ( 'NONE', #10753, #6962, #14537, .T. ) ;
#3625 = AXIS2_PLACEMENT_3D ( 'NONE', #2292, #3509, #5795 ) ;
#3626 = ADVANCED_FACE ( 'NONE', ( #7339 ), #1538, .F. ) ;
#3627 = CARTESIAN_POINT ( 'NONE',  ( -15.49969986081092088, -13.50737899243822504, 56.85231026484398598 ) ) ;
#3628 = DIRECTION ( 'NONE',  ( 0.8160499452489514693, 0.5779813897169900905, 3.090169943749478258E-16 ) ) ;
#3629 = CIRCLE ( 'NONE', #7028, 23.00000000000000000 ) ;
#3630 = AXIS2_PLACEMENT_3D ( 'NONE', #14209, #3730, #8387 ) ;
#3631 = CARTESIAN_POINT ( 'NONE',  ( -14.51048789653087390, -15.80334495249191207, 51.00231026484399166 ) ) ;
#3633 = LINE ( 'NONE', #10746, #9742 ) ;
#3632 = CARTESIAN_POINT ( 'NONE',  ( -7.512805849530849400, -44.04964101872660365, 19.96004823855532706 ) ) ;
#3634 = VECTOR ( 'NONE', #2338, 1000.000000000000114 ) ;
#3635 = ORIENTED_EDGE ( 'NONE', *, *, #13383, .T. ) ;
#3636 = CARTESIAN_POINT ( 'NONE',  ( -15.49969986081099194, -52.50737899243800655, 11.50231026484399521 ) ) ;
#3637 = DIRECTION ( 'NONE',  ( 0.000000000000000000, 1.000000000000000000, 1.224646799147350002E-16 ) ) ;
#3638 = VERTEX_POINT ( 'NONE', #14391 ) ;
#3639 = ORIENTED_EDGE ( 'NONE', *, *, #14282, .T. ) ;
#3640 = CARTESIAN_POINT ( 'NONE',  ( 21.93891671199435223, -29.45378376108857310, 22.06206851614466302 ) ) ;
#3641 = DIRECTION ( 'NONE',  ( -8.018662683283438208E-16, 5.975035461963189015E-16, 1.000000000000000000 ) ) ;
#3642 = ORIENTED_EDGE ( 'NONE', *, *, #4125, .F. ) ;
#3643 = AXIS2_PLACEMENT_3D ( 'NONE', #2437, #4733, #2508 ) ;
#3644 = FACE_OUTER_BOUND ( 'NONE', #7884, .T. ) ;
#3645 = AXIS2_PLACEMENT_3D ( 'NONE', #14248, #10142, #13603 ) ;
#3646 = EDGE_CURVE ( 'NONE', #3877, #10177, #3909, .T. ) ;
#3647 = EDGE_CURVE ( 'NONE', #6457, #1855, #2760, .T. ) ;
#3648 = EDGE_CURVE ( 'NONE', #14829, #14409, #12097, .T. ) ;
#3649 = CARTESIAN_POINT ( 'NONE',  ( 7.292741504061227786, 4.584400082011329758, 27.34761902326144423 ) ) ;
#3650 = DIRECTION ( 'NONE',  ( -5.000000000000000389E-16, 0.4999999999999998890, -0.8660254037844387076 ) ) ;
#3651 = AXIS2_PLACEMENT_3D ( 'NONE', #14061, #9694, #10773 ) ;
#3652 = EDGE_CURVE ( 'NONE', #8561, #1003, #10946, .T. ) ;
#3653 = CIRCLE ( 'NONE', #3907, 8.000000000000000000 ) ;
#3654 = DIRECTION ( 'NONE',  ( 8.018662683283438208E-16, -5.975035461963189015E-16, -1.000000000000000000 ) ) ;
#3655 = FACE_OUTER_BOUND ( 'NONE', #13669, .T. ) ;
#3656 = ORIENTED_EDGE ( 'NONE', *, *, #9346, .T. ) ;
#3657 = LINE ( 'NONE', #10769, #11907 ) ;
#3658 = CARTESIAN_POINT ( 'NONE',  ( -35.89930244329396913, 5.980169784832726876, 29.53939735812734568 ) ) ;
#3659 = ORIENTED_EDGE ( 'NONE', *, *, #12067, .T. ) ;
#3660 = PLANE ( 'NONE',  #3643 ) ;
#3661 = EDGE_LOOP ( 'NONE', ( #2550, #2751, #8218, #1733 ) ) ;
#3662 = CARTESIAN_POINT ( 'NONE',  ( -14.76203582817000104, -107.1622034095870077, -6.087689735155999315 ) ) ;
#3663 = VERTEX_POINT ( 'NONE', #13543 ) ;
#3664 = CARTESIAN_POINT ( 'NONE',  ( -9.989347722329670276, -49.50737899243800655, -5.497689735156000346 ) ) ;
#3665 = DIRECTION ( 'NONE',  ( 0.000000000000000000, -1.000000000000000000, -1.224646799147350002E-16 ) ) ;
#3666 = EDGE_CURVE ( 'NONE', #1380, #12994, #5909, .T. ) ;
#3667 = DIRECTION ( 'NONE',  ( 0.000000000000000000, 0.000000000000000000, 1.000000000000000000 ) ) ;
#3668 = VECTOR ( 'NONE', #7454, 1000.000000000000114 ) ;
#3669 = DIRECTION ( 'NONE',  ( 0.5975035461963188466, 0.8018662683283437342, 0.000000000000000000 ) ) ;
#3670 = DIRECTION ( 'NONE',  ( 0.000000000000000000, -1.850371707708594316E-16, 1.000000000000000000 ) ) ;
#3671 = CIRCLE ( 'NONE', #11001, 10.00000000000000000 ) ;
#3672 = CARTESIAN_POINT ( 'NONE',  ( 14.68618260102866913, -27.00737899243800300, 1.962064221501000683 ) ) ;
#3673 = EDGE_LOOP ( 'NONE', ( #10733, #9029, #12502, #6170 ) ) ;
#3674 = CARTESIAN_POINT ( 'NONE',  ( -9.661154126855418411, -49.98269403727269378, -17.54085436190861458 ) ) ;
#3675 = EDGE_CURVE ( 'NONE', #633, #8640, #12470, .T. ) ;
#3676 = CARTESIAN_POINT ( 'NONE',  ( -14.61203582817000246, -106.9373417306329515, -4.908392192767062845 ) ) ;
#3677 = ORIENTED_EDGE ( 'NONE', *, *, #638, .F. ) ;
#3678 = CARTESIAN_POINT ( 'NONE',  ( 7.392926877888857717, 4.291769771411865442, 21.97069516755205498 ) ) ;
#3679 = VERTEX_POINT ( 'NONE', #3052 ) ;
#3681 = ORIENTED_EDGE ( 'NONE', *, *, #3300, .F. ) ;
#3680 = LINE ( 'NONE', #14387, #10333 ) ;
#3682 = ORIENTED_EDGE ( 'NONE', *, *, #3453, .F. ) ;
#3683 = AXIS2_PLACEMENT_3D ( 'NONE', #6114, #8189, #12958 ) ;
#3684 = DIRECTION ( 'NONE',  ( 0.5975035461963189576, 0.8018662683283437342, 0.000000000000000000 ) ) ;
#3685 = ORIENTED_EDGE ( 'NONE', *, *, #10585, .F. ) ;
#3686 = CARTESIAN_POINT ( 'NONE',  ( -8.972439834930606040, -10.77678811232731348, 56.85231026484400019 ) ) ;
#3687 = DIRECTION ( 'NONE',  ( 3.632077277826439854E-16, -1.000000000000000000, 0.000000000000000000 ) ) ;
#3688 = LINE ( 'NONE', #4917, #12727 ) ;
#3689 = CARTESIAN_POINT ( 'NONE',  ( -7.528759897616733809, -14.80173833325270571, 57.00231026484399166 ) ) ;
#3690 = EDGE_CURVE ( 'NONE', #13117, #7160, #1985, .T. ) ;
#3691 = EDGE_CURVE ( 'NONE', #4357, #12241, #12024, .T. ) ;
#3692 = CYLINDRICAL_SURFACE ( 'NONE', #6398, 0.2500000000000004441 ) ;
#3693 = CARTESIAN_POINT ( 'NONE',  ( 2.660328366240848563, -40.75169664998565366, -13.30720238894809349 ) ) ;
#3694 = VERTEX_POINT ( 'NONE', #11315 ) ;
#3695 = DIRECTION ( 'NONE',  ( 1.000000000000000000, 0.000000000000000000, 0.000000000000000000 ) ) ;
#3696 = ORIENTED_EDGE ( 'NONE', *, *, #11102, .T. ) ;
#3697 = ORIENTED_EDGE ( 'NONE', *, *, #14916, .T. ) ;
#3698 = LINE ( 'NONE', #2551, #6621 ) ;
#3699 = EDGE_LOOP ( 'NONE', ( #52, #1076, #2530, #11521 ) ) ;
#3700 = DIRECTION ( 'NONE',  ( -0.8018662683283436232, 0.5975035461963189576, -9.999999999999996833E-16 ) ) ;
#3701 = CIRCLE ( 'NONE', #286, 9.974999999999999645 ) ;
#3702 = CARTESIAN_POINT ( 'NONE',  ( -7.064541492512761423, -18.83173137575486322, 57.00231026484399166 ) ) ;
#3703 = DIRECTION ( 'NONE',  ( 0.000000000000000000, -0.05233595624294329340, -0.9986295347545738332 ) ) ;
#3704 = CARTESIAN_POINT ( 'NONE',  ( -10.96448334217298282, -90.68610839286715475, -8.382549063897425157 ) ) ;
#3705 = AXIS2_PLACEMENT_3D ( 'NONE', #7577, #625, #14621 ) ;
#3706 = CARTESIAN_POINT ( 'NONE',  ( -15.39025577592761174, -21.58198560776530783, 56.85231026484400019 ) ) ;
#3707 = EDGE_CURVE ( 'NONE', #11022, #2020, #12317, .T. ) ;
#3709 = DIRECTION ( 'NONE',  ( 0.000000000000000000, 1.000000000000000000, 1.224646799147350002E-16 ) ) ;
#3708 = CARTESIAN_POINT ( 'NONE',  ( -21.48581293389290892, -5.528213918555016981, 54.00231026484397745 ) ) ;
#3710 = ORIENTED_EDGE ( 'NONE', *, *, #11703, .F. ) ;
#3711 = CYLINDRICAL_SURFACE ( 'NONE', #7511, 0.2500000000000004441 ) ;
#3712 = DIRECTION ( 'NONE',  ( 1.000000000000000000, 1.201369187114119994E-15, 9.616040805000176517E-16 ) ) ;
#3713 = ORIENTED_EDGE ( 'NONE', *, *, #7358, .T. ) ;
#3714 = VERTEX_POINT ( 'NONE', #2138 ) ;
#3715 = CARTESIAN_POINT ( 'NONE',  ( 21.86822340939376019, -27.85492751190550109, 27.35691555891743221 ) ) ;
#3716 = LINE ( 'NONE', #11741, #9090 ) ;
#3717 = ORIENTED_EDGE ( 'NONE', *, *, #11375, .T. ) ;
#3718 = CARTESIAN_POINT ( 'NONE',  ( -7.706583154360178156, -42.68076247385797473, -17.17902169384817057 ) ) ;
#3719 = VECTOR ( 'NONE', #877, 1000.000000000000114 ) ;
#3720 = AXIS2_PLACEMENT_3D ( 'NONE', #7584, #6206, #6283 ) ;
#3721 = AXIS2_PLACEMENT_3D ( 'NONE', #13676, #6615, #6394 ) ;
#3722 = LINE ( 'NONE', #1270, #10497 ) ;
#3723 = FACE_OUTER_BOUND ( 'NONE', #1749, .T. ) ;
#3724 = CARTESIAN_POINT ( 'NONE',  ( -7.593867891459233910, -45.75082787501852977, 17.08720858567314238 ) ) ;
#3725 = ADVANCED_FACE ( 'NONE', ( #1913 ), #6708, .F. ) ;
#3726 = DIRECTION ( 'NONE',  ( 0.9826409426582665141, -0.1855175943453169496, 8.987940462991673516E-16 ) ) ;
#3727 = ORIENTED_EDGE ( 'NONE', *, *, #11931, .F. ) ;
#3728 = DIRECTION ( 'NONE',  ( 1.000000000000000000, 3.700743415417188632E-16, 0.000000000000000000 ) ) ;
#3729 = VECTOR ( 'NONE', #1834, 1000.000000000000114 ) ;
#3730 = DIRECTION ( 'NONE',  ( 0.4177292884839972631, 0.9085715390340232123, -2.079116908177589032E-16 ) ) ;
#3731 = EDGE_LOOP ( 'NONE', ( #13094, #1257, #15047, #12883 ) ) ;
#3732 = VECTOR ( 'NONE', #9879, 999.9999999999998863 ) ;
#3733 = EDGE_CURVE ( 'NONE', #13947, #13156, #4109, .T. ) ;
#3734 = FACE_OUTER_BOUND ( 'NONE', #4223, .T. ) ;
#3735 = ORIENTED_EDGE ( 'NONE', *, *, #8990, .T. ) ;
#3736 = CARTESIAN_POINT ( 'NONE',  ( -7.497191992632178170, -44.39045585651064840, -6.841238297419723224 ) ) ;
#3737 = ORIENTED_EDGE ( 'NONE', *, *, #303, .F. ) ;
#3738 = DIRECTION ( 'NONE',  ( 0.000000000000000000, 1.224646799147350002E-16, -1.000000000000000000 ) ) ;
#3739 = CARTESIAN_POINT ( 'NONE',  ( -15.49969986081100615, -101.3912783891275069, -6.049618808461761255 ) ) ;
#3740 = EDGE_CURVE ( 'NONE', #14164, #7674, #13744, .T. ) ;
#3741 = CARTESIAN_POINT ( 'NONE',  ( -35.80601265084419538, 12.32432269366989530, 16.16206422150100153 ) ) ;
#3742 = CARTESIAN_POINT ( 'NONE',  ( -15.49969986081099904, 20.99262100756200056, 24.21206422150099868 ) ) ;
#3743 = AXIS2_PLACEMENT_3D ( 'NONE', #14080, #12017, #11781 ) ;
#3744 = LINE ( 'NONE', #1370, #4076 ) ;
#3745 = CARTESIAN_POINT ( 'NONE',  ( 17.35862657855726354, -30.12898149287163108, 6.139218436208705221 ) ) ;
#3746 = EDGE_CURVE ( 'NONE', #10582, #14123, #308, .T. ) ;
#3747 = ORIENTED_EDGE ( 'NONE', *, *, #10894, .F. ) ;
#3748 = CARTESIAN_POINT ( 'NONE',  ( -11.27121226320114644, -51.30363337802549495, -17.75917625400039057 ) ) ;
#3749 = EDGE_CURVE ( 'NONE', #7451, #14647, #4458, .T. ) ;
#3750 = CARTESIAN_POINT ( 'NONE',  ( -15.49969986081092088, -13.50737899243822504, 57.00231026484397745 ) ) ;
#3751 = CARTESIAN_POINT ( 'NONE',  ( -20.18599136182623965, -52.50737899243802786, 2.502310264844031185 ) ) ;
#3752 = ORIENTED_EDGE ( 'NONE', *, *, #14899, .F. ) ;
#3753 = CARTESIAN_POINT ( 'NONE',  ( -15.49969986081092088, -13.50737899243822504, 57.00231026484397745 ) ) ;
#3754 = ORIENTED_EDGE ( 'NONE', *, *, #1447, .F. ) ;
#3756 = ORIENTED_EDGE ( 'NONE', *, *, #4019, .T. ) ;
#3755 = DIRECTION ( 'NONE',  ( 0.000000000000000000, 0.1872998510044689147, 0.9823027872370635460 ) ) ;
#3757 = ORIENTED_EDGE ( 'NONE', *, *, #9847, .T. ) ;
#3758 = AXIS2_PLACEMENT_3D ( 'NONE', #4276, #13688, #3127 ) ;
#3759 = DIRECTION ( 'NONE',  ( -8.018662683283438208E-16, 5.975035461963189015E-16, 1.000000000000000000 ) ) ;
#3760 = AXIS2_PLACEMENT_3D ( 'NONE', #13906, #1202, #2431 ) ;
#3761 = EDGE_LOOP ( 'NONE', ( #12177, #5435, #167, #13592 ) ) ;
#3762 = LINE ( 'NONE', #8418, #1934 ) ;
#3763 = CARTESIAN_POINT ( 'NONE',  ( -35.18530787408279537, 11.99262100756689620, 16.16206422150100153 ) ) ;
#3764 = PLANE ( 'NONE',  #751 ) ;
#3765 = CARTESIAN_POINT ( 'NONE',  ( -11.58094331127308507, -5.879823872646938732, 56.85231026484398598 ) ) ;
#3766 = AXIS2_PLACEMENT_3D ( 'NONE', #11641, #2468, #5822 ) ;
#3767 = ADVANCED_FACE ( 'NONE', ( #843 ), #10081, .F. ) ;
#3768 = DIRECTION ( 'NONE',  ( 0.9354976265738682573, -0.3533329742249642913, 9.612616959383187437E-16 ) ) ;
#3769 = CARTESIAN_POINT ( 'NONE',  ( -23.49646891012291050, -9.216349422280851300, 56.85231026484398598 ) ) ;
#3770 = ORIENTED_EDGE ( 'NONE', *, *, #9725, .F. ) ;
#3771 = DIRECTION ( 'NONE',  ( 8.018662683283438208E-16, -5.975035461963189015E-16, -1.000000000000000000 ) ) ;
#3772 =( NAMED_UNIT ( * ) PLANE_ANGLE_UNIT ( ) SI_UNIT ( $, .RADIAN. ) );
#3773 = CIRCLE ( 'NONE', #5716, 9.974999999999999645 ) ;
#3774 = EDGE_LOOP ( 'NONE', ( #13158, #5808 ) ) ;
#3775 = ORIENTED_EDGE ( 'NONE', *, *, #4019, .F. ) ;
#3776 = LINE ( 'NONE', #10657, #8088 ) ;
#3777 = EDGE_LOOP ( 'NONE', ( #14658, #12854, #13022, #1711 ) ) ;
#3778 = FACE_OUTER_BOUND ( 'NONE', #14022, .T. ) ;
#3779 = CARTESIAN_POINT ( 'NONE',  ( -17.02073322366946684, -23.42091518255481475, 56.97733164403681627 ) ) ;
#3780 = VECTOR ( 'NONE', #6923, 1000.000000000000000 ) ;
#3781 = EDGE_CURVE ( 'NONE', #14193, #11181, #5498, .T. ) ;
#3782 = CYLINDRICAL_SURFACE ( 'NONE', #10964, 2.500000000000002220 ) ;
#3783 = DIRECTION ( 'NONE',  ( 8.018662683283438208E-16, -5.975035461963189015E-16, -1.000000000000000000 ) ) ;
#3784 = VECTOR ( 'NONE', #14798, 1000.000000000000000 ) ;
#3786 = CARTESIAN_POINT ( 'NONE',  ( -38.20013690429809827, 4.873818854045000037, 27.91208557747711083 ) ) ;
#3785 = CARTESIAN_POINT ( 'NONE',  ( -7.499960972858381147, -49.00661531336379539, -5.561496955626357597 ) ) ;
#3787 = ORIENTED_EDGE ( 'NONE', *, *, #7190, .F. ) ;
#3788 = DIRECTION ( 'NONE',  ( -0.9957106782009863544, -0.09252159378508259535, -7.431448254773871651E-16 ) ) ;
#3789 = CARTESIAN_POINT ( 'NONE',  ( -7.758527451664999575, -46.50737899243799944, -5.497689735156000346 ) ) ;
#3790 = ORIENTED_EDGE ( 'NONE', *, *, #4522, .F. ) ;
#3791 = VERTEX_POINT ( 'NONE', #8937 ) ;
#3792 = CARTESIAN_POINT ( 'NONE',  ( 21.91137017292814093, -28.99035275200779083, 21.62826645491238509 ) ) ;
#3793 = CARTESIAN_POINT ( 'NONE',  ( -19.68577560955674954, -20.41303028871448788, 56.85231026484398598 ) ) ;
#3794 = ORIENTED_EDGE ( 'NONE', *, *, #6847, .F. ) ;
#3795 = CARTESIAN_POINT ( 'NONE',  ( -7.924984455289715513, -41.92032950385904400, -17.22478920316331852 ) ) ;
#3796 = EDGE_CURVE ( 'NONE', #14198, #10750, #5665, .T. ) ;
#3797 = DIRECTION ( 'NONE',  ( -8.018662683283438208E-16, 5.975035461963189015E-16, 1.000000000000000000 ) ) ;
#3798 = CARTESIAN_POINT ( 'NONE',  ( -9.290890585402740598, -21.34661493808534516, 56.48450469233716120 ) ) ;
#3799 = CARTESIAN_POINT ( 'NONE',  ( -15.49969986081099904, 7.183219930803497633, 24.21206422150099868 ) ) ;
#3800 = FACE_OUTER_BOUND ( 'NONE', #13614, .T. ) ;
#3801 = ORIENTED_EDGE ( 'NONE', *, *, #13922, .F. ) ;
#3802 = CARTESIAN_POINT ( 'NONE',  ( -9.539601987502637215, -5.508762965862999295, 54.00231026484399166 ) ) ;
#3803 = CARTESIAN_POINT ( 'NONE',  ( -5.499699860810997265, -46.50737899243799944, -5.497689735156003010 ) ) ;
#3804 = ORIENTED_EDGE ( 'NONE', *, *, #1571, .F. ) ;
#3805 = CARTESIAN_POINT ( 'NONE',  ( -7.497885806132468467, -44.50611869254105102, 18.00659976627173720 ) ) ;
#3806 = ORIENTED_EDGE ( 'NONE', *, *, #7802, .T. ) ;
#3807 = AXIS2_PLACEMENT_3D ( 'NONE', #8775, #14974, #4424 ) ;
#3808 = DIRECTION ( 'NONE',  ( -8.018662683283438208E-16, 5.975035461963189015E-16, 1.000000000000000000 ) ) ;
#3809 = ORIENTED_EDGE ( 'NONE', *, *, #4279, .T. ) ;
#3810 = DIRECTION ( 'NONE',  ( 0.000000000000000000, -1.508455196501571676E-16, 1.000000000000000000 ) ) ;
#3811 = FACE_OUTER_BOUND ( 'NONE', #7617, .T. ) ;
#3812 = EDGE_CURVE ( 'NONE', #12430, #2788, #10155, .T. ) ;
#3813 = DIRECTION ( 'NONE',  ( 0.000000000000000000, 1.000000000000000000, 1.224646799147350002E-16 ) ) ;
#3814 = EDGE_CURVE ( 'NONE', #14904, #4847, #5645, .T. ) ;
#3815 = CARTESIAN_POINT ( 'NONE',  ( -15.49969986081099194, -57.00737899243800655, 19.50231026484399521 ) ) ;
#3816 = AXIS2_PLACEMENT_3D ( 'NONE', #8018, #11696, #9246 ) ;
#3817 = ORIENTED_EDGE ( 'NONE', *, *, #3515, .F. ) ;
#3818 = DIRECTION ( 'NONE',  ( -0.8415927028326188886, 0.5401126942952620968, -9.975640502598240034E-16 ) ) ;
#3819 = CARTESIAN_POINT ( 'NONE',  ( -34.28383802683607939, -39.31204358973022295, 51.95868366853013498 ) ) ;
#3820 = CARTESIAN_POINT ( 'NONE',  ( -15.49969986081099904, 2.992621007561997004, 24.21206422150099868 ) ) ;
#3821 = ORIENTED_EDGE ( 'NONE', *, *, #11967, .F. ) ;
#3822 = DIRECTION ( 'NONE',  ( 0.5975035461963189576, 0.8018662683283437342, 0.000000000000000000 ) ) ;
#3823 = ORIENTED_EDGE ( 'NONE', *, *, #5707, .F. ) ;
#3825 = ORIENTED_EDGE ( 'NONE', *, *, #2453, .F. ) ;
#3824 = DIRECTION ( 'NONE',  ( 8.018662683283438208E-16, -5.975035461963189015E-16, -1.000000000000000000 ) ) ;
#3826 = ORIENTED_EDGE ( 'NONE', *, *, #6229, .T. ) ;
#3827 = LINE ( 'NONE', #10874, #8606 ) ;
#3828 = VECTOR ( 'NONE', #7640, 1000.000000000000114 ) ;
#3829 = DIRECTION ( 'NONE',  ( 1.084202172485505026E-15, -0.1872998510044511788, -0.9823027872370668767 ) ) ;
#3830 = EDGE_CURVE ( 'NONE', #4342, #7312, #8837, .T. ) ;
#3831 = EDGE_CURVE ( 'NONE', #11437, #3470, #14472, .T. ) ;
#3832 = DIRECTION ( 'NONE',  ( -0.9645173894937585368, -0.2640193276336892936, -6.156614753256587028E-16 ) ) ;
#3833 = VECTOR ( 'NONE', #2244, 1000.000000000000000 ) ;
#3834 = CARTESIAN_POINT ( 'NONE',  ( -17.61203582816999713, -107.4899781488447985, -7.806719612820868903 ) ) ;
#3835 = PRODUCT_CONTEXT ( 'NONE', #5084, 'mechanical' ) ;
#3836 = CARTESIAN_POINT ( 'NONE',  ( -15.79707957972810384, -9.007378992438001220, -13.28793577849899599 ) ) ;
#3837 = AXIS2_PLACEMENT_3D ( 'NONE', #1529, #10706, #5954 ) ;
#3838 = EDGE_CURVE ( 'NONE', #11680, #8983, #13992, .T. ) ;
#3839 = DIRECTION ( 'NONE',  ( -0.2640193276336892936, 0.9645173894937585368, -7.880107536067216805E-16 ) ) ;
#3840 = DIRECTION ( 'NONE',  ( -8.018662683283438208E-16, 5.975035461963189015E-16, 1.000000000000000000 ) ) ;
#3841 = ORIENTED_EDGE ( 'NONE', *, *, #6744, .T. ) ;
#3842 = CARTESIAN_POINT ( 'NONE',  ( -15.49969986081099904, 70.81438635534659909, 24.21206422150100579 ) ) ;
#3843 = EDGE_LOOP ( 'NONE', ( #498, #11722, #5179, #7153 ) ) ;
#3844 = EDGE_LOOP ( 'NONE', ( #1152, #14832, #113, #867 ) ) ;
#3845 = CARTESIAN_POINT ( 'NONE',  ( -15.49969986081092621, -96.50737899243799234, -9.210188241073819171 ) ) ;
#3846 = ORIENTED_EDGE ( 'NONE', *, *, #3157, .T. ) ;
#3847 = ORIENTED_EDGE ( 'NONE', *, *, #4215, .F. ) ;
#3848 = CARTESIAN_POINT ( 'NONE',  ( -15.61203582816999891, -108.1070660607018397, -6.416813587133916919 ) ) ;
#3849 = CARTESIAN_POINT ( 'NONE',  ( -21.11416342254291934, -20.63752968607602867, 56.85231026484398598 ) ) ;
#3850 = ADVANCED_FACE ( 'NONE', ( #12932 ), #7003, .T. ) ;
#3851 = VECTOR ( 'NONE', #13447, 1000.000000000000114 ) ;
#3852 = SURFACE_STYLE_USAGE ( .BOTH. , #1485 ) ;
#3853 = AXIS2_PLACEMENT_3D ( 'NONE', #8031, #3148, #5514 ) ;
#3854 = CARTESIAN_POINT ( 'NONE',  ( -11.91715604007085716, -91.02193864445173688, -9.500011814598602555 ) ) ;
#3855 = CARTESIAN_POINT ( 'NONE',  ( -15.49969986081094042, -85.00737899243800655, -5.497689735156000346 ) ) ;
#3857 = CARTESIAN_POINT ( 'NONE',  ( -14.61203582816999891, -107.3260907792159031, -6.947204673988433221 ) ) ;
#3856 = LINE ( 'NONE', #8518, #11274 ) ;
#3858 = EDGE_LOOP ( 'NONE', ( #4639, #5418, #1514, #4219 ) ) ;
#3859 = CARTESIAN_POINT ( 'NONE',  ( -15.16333526000374476, -10.64029123852186665, 51.10586365543726117 ) ) ;
#3860 = VECTOR ( 'NONE', #3161, 1000.000000000000000 ) ;
#3861 = DIRECTION ( 'NONE',  ( 0.04695496274984587576, 0.9988970074402868660, -5.591929034707467802E-16 ) ) ;
#3862 = ORIENTED_EDGE ( 'NONE', *, *, #8128, .F. ) ;
#3863 = VERTEX_POINT ( 'NONE', #13004 ) ;
#3864 = CARTESIAN_POINT ( 'NONE',  ( 21.97302893587540851, -29.92705860424354825, 22.76870634099842761 ) ) ;
#3865 = ADVANCED_FACE ( 'NONE', ( #9398 ), #2291, .F. ) ;
#3866 = AXIS2_PLACEMENT_3D ( 'NONE', #4738, #10393, #15061 ) ;
#3867 = CIRCLE ( 'NONE', #6531, 8.886381701226328644 ) ;
#3868 = LINE ( 'NONE', #14048, #13011 ) ;
#3869 = FACE_OUTER_BOUND ( 'NONE', #11652, .T. ) ;
#3870 = VERTEX_POINT ( 'NONE', #11543 ) ;
#3871 = CARTESIAN_POINT ( 'NONE',  ( -22.55857771067089246, -13.99059064457067336, 56.85231026484398598 ) ) ;
#3872 = B_SPLINE_CURVE_WITH_KNOTS ( 'NONE', 3,
 ( #7453, #6594, #13509, #9976, #6451, #5164, #12287, #12358, #582, #4171, #12130, #2800, #2948, #14651, #8751, #1647, #10044, #9837, #11059 ),
 .UNSPECIFIED., .F., .F.,
 ( 4, 2, 2, 2, 1, 1, 1, 1, 1, 2, 2, 4 ),
 ( 0.000000000000000000, 0.2500000000000998090, 0.3750000000001501577, 0.4375000000001756373, 0.4687500000001887379, 0.4843750000001955658, 0.4921875000001992295, 0.4960937500002022826, 0.4980468750002025602, 0.4990234375002016720, 0.5000000000002008393, 1.000000000000000000 ),
 .UNSPECIFIED. ) ;
#3873 = DIRECTION ( 'NONE',  ( 0.000000000000000000, 0.1872998510044759646, 0.9823027872370621028 ) ) ;
#3874 = CARTESIAN_POINT ( 'NONE',  ( -7.959143533992851793, -20.11997055668047096, 56.24285220617511527 ) ) ;
#3875 = DIRECTION ( 'NONE',  ( 0.5975035461963188466, 0.8018662683283437342, 0.000000000000000000 ) ) ;
#3876 = CARTESIAN_POINT ( 'NONE',  ( -19.27841348868324189, -22.73895244004356897, 54.00231026484399166 ) ) ;
#3877 = VERTEX_POINT ( 'NONE', #9164 ) ;
#3878 = LINE ( 'NONE', #1357, #3358 ) ;
#3879 = CYLINDRICAL_SURFACE ( 'NONE', #11413, 8.000000000000003553 ) ;
#3880 = VERTEX_POINT ( 'NONE', #151 ) ;
#3881 = B_SPLINE_CURVE_WITH_KNOTS ( 'NONE', 3,
 ( #6450, #13583, #578, #11133, #5244, #649, #7747, #5313, #4169, #14220, #7896, #13655, #11277, #5533, #10120, #5760, #14945, #13804, #14876, #10279, #13726, #11430, #4320, #7815, #6827, #11356 ),
 .UNSPECIFIED., .F., .F.,
 ( 4, 2, 2, 2, 2, 2, 2, 2, 2, 2, 2, 2, 4 ),
 ( 0.02522177263268702771, 0.02600995928983864530, 0.02679814594699025943, 0.02837451926129350155, 0.02916270591844511567, 0.02995089257559673326, 0.03152726588989995804, 0.03231545254705157216, 0.03310363920420318629, 0.03389182586135480041, 0.03468001251850641453, 0.03625638583280965666, 0.03783275914711289878 ),
 .UNSPECIFIED. ) ;
#3882 = AXIS2_PLACEMENT_3D ( 'NONE', #9366, #5833, #14264 ) ;
#3883 = EDGE_CURVE ( 'NONE', #4490, #415, #10471, .T. ) ;
#3884 = CARTESIAN_POINT ( 'NONE',  ( -7.502372241906894779, -44.29399517289605370, 18.32448191336956000 ) ) ;
#3885 = LINE ( 'NONE', #9695, #7241 ) ;
#3886 = ORIENTED_EDGE ( 'NONE', *, *, #8276, .T. ) ;
#3887 = DIRECTION ( 'NONE',  ( 0.9755678736739574752, -0.2196982563774083075, 9.135454576426028331E-16 ) ) ;
#3888 = ORIENTED_EDGE ( 'NONE', *, *, #12738, .F. ) ;
#3889 = DIRECTION ( 'NONE',  ( 0.5975035461963189576, 0.8018662683283437342, 0.000000000000000000 ) ) ;
#3890 = DIRECTION ( 'NONE',  ( 1.000000000000000000, 0.000000000000000000, 0.000000000000000000 ) ) ;
#3891 = CARTESIAN_POINT ( 'NONE',  ( 22.00030013918900096, -27.00737899243800300, 1.962064221501000683 ) ) ;
#3892 = VECTOR ( 'NONE', #12331, 1000.000000000000227 ) ;
#3893 = PRODUCT_DEFINITION_FORMATION_WITH_SPECIFIED_SOURCE ( 'ANY', '', #4461, .NOT_KNOWN. ) ;
#3894 = CARTESIAN_POINT ( 'NONE',  ( -7.506424547597140950, -48.98717474752370293, 19.17796694551992687 ) ) ;
#3895 = CARTESIAN_POINT ( 'NONE',  ( 17.85498670612308914, -29.68038497774185558, 7.072740731940803549 ) ) ;
#3896 = DIRECTION ( 'NONE',  ( -8.018662683283438208E-16, 5.975035461963189015E-16, 1.000000000000000000 ) ) ;
#3897 = ORIENTED_EDGE ( 'NONE', *, *, #14678, .F. ) ;
#3898 = CARTESIAN_POINT ( 'NONE',  ( -7.499699860810997265, -45.03775106554863328, -17.13441993860075030 ) ) ;
#3899 = CARTESIAN_POINT ( 'NONE',  ( -34.67966921736225316, -38.76197583040457317, 51.72704121311384995 ) ) ;
#3900 = EDGE_CURVE ( 'NONE', #6722, #13722, #9238, .T. ) ;
#3901 = ORIENTED_EDGE ( 'NONE', *, *, #3157, .F. ) ;
#3902 = DIRECTION ( 'NONE',  ( 0.3857661296576155308, 0.9225966037272105291, -2.419218955996680478E-16 ) ) ;
#3903 = ORIENTED_EDGE ( 'NONE', *, *, #2454, .T. ) ;
#3905 = ORIENTED_EDGE ( 'NONE', *, *, #11548, .F. ) ;
#3904 = LINE ( 'NONE', #6105, #11070 ) ;
#3906 = EDGE_LOOP ( 'NONE', ( #3806, #1964, #14003, #1744 ) ) ;
#3907 = AXIS2_PLACEMENT_3D ( 'NONE', #2722, #13143, #285 ) ;
#3908 = EDGE_CURVE ( 'NONE', #3526, #9567, #10392, .T. ) ;
#3909 = LINE ( 'NONE', #13397, #11788 ) ;
#3910 = CARTESIAN_POINT ( 'NONE',  ( -15.49969986081099904, -13.50737899243800122, 48.00231026484399877 ) ) ;
#3911 = DIRECTION ( 'NONE',  ( 0.9805849309054467389, 0.1960948578651675878, 6.691306063588567679E-16 ) ) ;
#3912 = CARTESIAN_POINT ( 'NONE',  ( -12.46042140754850180, -23.00808483377099734, 56.85231026484400019 ) ) ;
#3913 = SHAPE_DEFINITION_REPRESENTATION ( #13378, #6151 ) ;
#3914 = CARTESIAN_POINT ( 'NONE',  ( -16.84408283975263032, -15.31157809617700316, 51.25231026484399166 ) ) ;
#3915 = CARTESIAN_POINT ( 'NONE',  ( -7.510307729924003084, -44.09336537972112779, 43.83865520846783426 ) ) ;
#3916 = EDGE_CURVE ( 'NONE', #15033, #4751, #1063, .T. ) ;
#3917 = LINE ( 'NONE', #13188, #57 ) ;
#3918 = CIRCLE ( 'NONE', #14176, 9.974999999999999645 ) ;
#3919 = ORIENTED_EDGE ( 'NONE', *, *, #3069, .T. ) ;
#3920 = DIRECTION ( 'NONE',  ( -0.9578660637129379207, 0.2872152572324145892, -9.396926207859088029E-16 ) ) ;
#3921 = DIRECTION ( 'NONE',  ( -8.018662683283438208E-16, 5.975035461963189015E-16, 1.000000000000000000 ) ) ;
#3922 = ORIENTED_EDGE ( 'NONE', *, *, #13048, .T. ) ;
#3923 = ORIENTED_EDGE ( 'NONE', *, *, #6157, .T. ) ;
#3924 = ADVANCED_FACE ( 'NONE', ( #13840, #1212 ), #3356, .F. ) ;
#3925 = FACE_OUTER_BOUND ( 'NONE', #5332, .T. ) ;
#3926 = ORIENTED_EDGE ( 'NONE', *, *, #7753, .F. ) ;
#3927 = CARTESIAN_POINT ( 'NONE',  ( -16.38999062866295020, -11.44100962838991364, 51.25231026484399166 ) ) ;
#3928 = EDGE_CURVE ( 'NONE', #1378, #9153, #11761, .T. ) ;
#3929 = DIRECTION ( 'NONE',  ( 0.000000000000000000, 1.000000000000000000, 1.224646799147350002E-16 ) ) ;
#3930 = LINE ( 'NONE', #9960, #9746 ) ;
#3931 = SHAPE_REPRESENTATION ( 'Slide Locking Screw', ( #6789 ), #8516 ) ;
#3932 = FACE_OUTER_BOUND ( 'NONE', #2919, .T. ) ;
#3934 = CARTESIAN_POINT ( 'NONE',  ( -36.49062000465940514, 5.696595093598766368, 19.22546363248600088 ) ) ;
#3933 = CARTESIAN_POINT ( 'NONE',  ( -14.99866629829804765, -4.445910272123860807, 56.85231026484398598 ) ) ;
#3935 = ADVANCED_FACE ( 'NONE', ( #11845, #9468 ), #5944, .T. ) ;
#3936 = EDGE_LOOP ( 'NONE', ( #10642, #11417, #10270, #13817 ) ) ;
#3937 = DIRECTION ( 'NONE',  ( 3.202566417187950042E-16, 1.224646799147350002E-16, -1.000000000000000000 ) ) ;
#3938 = EDGE_CURVE ( 'NONE', #9118, #14007, #5864, .T. ) ;
#3939 = ORIENTED_EDGE ( 'NONE', *, *, #12976, .T. ) ;
#3940 = CARTESIAN_POINT ( 'NONE',  ( -25.15786752016616035, -16.15135352813856073, 60.44742509602125580 ) ) ;
#3941 = VERTEX_POINT ( 'NONE', #8166 ) ;
#3942 = ORIENTED_EDGE ( 'NONE', *, *, #11284, .T. ) ;
#3943 = CARTESIAN_POINT ( 'NONE',  ( -12.23206416678372577, -4.082773856353239417, 54.00231026484399166 ) ) ;
#3944 = DIRECTION ( 'NONE',  ( 0.4587843131450244361, -0.8885476655824651182, 8.987940462991667599E-16 ) ) ;
#3945 = ORIENTED_EDGE ( 'NONE', *, *, #8691, .T. ) ;
#3946 = LINE ( 'NONE', #1878, #5609 ) ;
#3947 = VECTOR ( 'NONE', #10108, 1000.000000000000000 ) ;
#3948 = DIRECTION ( 'NONE',  ( 0.5975035461963189576, 0.8018662683283437342, 0.000000000000000000 ) ) ;
#3949 = DIRECTION ( 'NONE',  ( -8.018662683283438208E-16, 5.975035461963189015E-16, 1.000000000000000000 ) ) ;
#3950 = FACE_OUTER_BOUND ( 'NONE', #9390, .T. ) ;
#3951 = ORIENTED_EDGE ( 'NONE', *, *, #6046, .T. ) ;
#3952 = CARTESIAN_POINT ( 'NONE',  ( -14.61203582817000246, -107.1621692949231317, -5.034900018422283630 ) ) ;
#3953 = LINE ( 'NONE', #217, #10181 ) ;
#3954 = EDGE_LOOP ( 'NONE', ( #7614, #10618, #13800, #1479 ) ) ;
#3955 = AXIS2_PLACEMENT_3D ( 'NONE', #7353, #6207, #6430 ) ;
#3956 = EDGE_CURVE ( 'NONE', #12928, #818, #4659, .T. ) ;
#3957 = LINE ( 'NONE', #2811, #5907 ) ;
#3958 = SURFACE_STYLE_USAGE ( .BOTH. , #9543 ) ;
#3959 = EDGE_LOOP ( 'NONE', ( #7599, #12679, #9463, #10080 ) ) ;
#3960 = CARTESIAN_POINT ( 'NONE',  ( -15.49969986081092088, -13.50737899243822504, 57.00231026484397745 ) ) ;
#3961 = ORIENTED_EDGE ( 'NONE', *, *, #5810, .F. ) ;
#3962 = CARTESIAN_POINT ( 'NONE',  ( -7.886584594865169606, -46.96511696614940234, 21.96004823855531640 ) ) ;
#3963 = VECTOR ( 'NONE', #14471, 1000.000000000000000 ) ;
#3964 = PRODUCT_DEFINITION_SHAPE ( 'NONE', 'NONE',  #15127 ) ;
#3965 = CARTESIAN_POINT ( 'NONE',  ( -15.49969986081099904, -2.007378992438000331, 24.21206422150100224 ) ) ;
#3966 = EDGE_CURVE ( 'NONE', #1260, #6753, #10102, .T. ) ;
#3967 = CARTESIAN_POINT ( 'NONE',  ( -7.797100586692807589, -47.75470106918052693, 17.33567862706513552 ) ) ;
#3968 = VECTOR ( 'NONE', #2194, 1000.000000000000114 ) ;
#3969 = VECTOR ( 'NONE', #14833, 1000.000000000000114 ) ;
#3970 = CIRCLE ( 'NONE', #4950, 6.000000000000000000 ) ;
#3971 = VECTOR ( 'NONE', #3587, 1000.000000000000000 ) ;
#3972 = CARTESIAN_POINT ( 'NONE',  ( 14.95806614058027861, -28.53604795622425527, 2.335433060012842343 ) ) ;
#3973 = LINE ( 'NONE', #14380, #7903 ) ;
#3974 = ORIENTED_EDGE ( 'NONE', *, *, #13552, .T. ) ;
#3975 = CARTESIAN_POINT ( 'NONE',  ( -19.51793069539949599, -6.502732608789604463, 56.85231026484398598 ) ) ;
#3976 = DIRECTION ( 'NONE',  ( 0.000000000000000000, -1.000000000000000000, -1.224646799147350002E-16 ) ) ;
#3977 = ORIENTED_EDGE ( 'NONE', *, *, #8963, .T. ) ;
#3978 = ORIENTED_EDGE ( 'NONE', *, *, #12529, .T. ) ;
#3980 = ORIENTED_EDGE ( 'NONE', *, *, #8611, .F. ) ;
#3979 = CYLINDRICAL_SURFACE ( 'NONE', #13529, 22.99999999999999645 ) ;
#3981 = ORIENTED_EDGE ( 'NONE', *, *, #10600, .F. ) ;
#3982 = CARTESIAN_POINT ( 'NONE',  ( -7.829332545557824652, -7.130382030772257629, 57.00231026484399166 ) ) ;
#3983 = CARTESIAN_POINT ( 'NONE',  ( 2.500300139189001847, -46.50737899243799944, -5.497689735156002122 ) ) ;
#3984 = VECTOR ( 'NONE', #7527, 1000.000000000000000 ) ;
#3985 = CARTESIAN_POINT ( 'NONE',  ( -18.18846581869434686, -17.11577719991577595, 46.00231026484398456 ) ) ;
#3986 = EDGE_CURVE ( 'NONE', #3051, #6590, #3583, .T. ) ;
#3987 = CARTESIAN_POINT ( 'NONE',  ( -13.22804965902115093, -3.767132336032069428, 61.64459019995985756 ) ) ;
#3988 = LINE ( 'NONE', #5136, #15098 ) ;
#3989 = VECTOR ( 'NONE', #11257, 1000.000000000000000 ) ;
#3990 = CARTESIAN_POINT ( 'NONE',  ( -7.514630092986283039, -44.01837396645046141, 44.23252331109035396 ) ) ;
#3991 = CARTESIAN_POINT ( 'NONE',  ( -15.49969986081099904, 1010.738102757665615, 1688.491546572001198 ) ) ;
#3992 = AXIS2_PLACEMENT_3D ( 'NONE', #5323, #12439, #1958 ) ;
#3993 = VECTOR ( 'NONE', #5767, 1000.000000000000000 ) ;
#3994 = ORIENTED_EDGE ( 'NONE', *, *, #6485, .T. ) ;
#3995 = PLANE ( 'NONE',  #6322 ) ;
#3996 = ORIENTED_EDGE ( 'NONE', *, *, #177, .F. ) ;
#3997 = ORIENTED_EDGE ( 'NONE', *, *, #2655, .F. ) ;
#3998 = LINE ( 'NONE', #8030, #11039 ) ;
#3999 = CARTESIAN_POINT ( 'NONE',  ( -15.49969986081099549, 2.992621007561994340, 47.21206422150099513 ) ) ;
#4000 = EDGE_LOOP ( 'NONE', ( #6740, #14277 ) ) ;
#4001 = CARTESIAN_POINT ( 'NONE',  ( -11.14367517063017310, -12.33997039914164517, -13.03412254519544433 ) ) ;
#4002 = CIRCLE ( 'NONE', #10839, 2.499999999999999556 ) ;
#4003 = EDGE_CURVE ( 'NONE', #612, #3870, #5794, .T. ) ;
#4004 = CARTESIAN_POINT ( 'NONE',  ( -31.79969986081099975, 20.99262100756200056, 16.16206422150100153 ) ) ;
#4005 = DIRECTION ( 'NONE',  ( 1.000000000000000000, 0.000000000000000000, 0.000000000000000000 ) ) ;
#4006 = ADVANCED_FACE ( 'NONE', ( #11207 ), #14573, .T. ) ;
#4007 = APPLICATION_CONTEXT ( 'automotive_design' ) ;
#4008 = AXIS2_PLACEMENT_3D ( 'NONE', #10969, #9308, #13984 ) ;
#4010 = CARTESIAN_POINT ( 'NONE',  ( -35.93898377820745083, 5.961151497827927415, 18.90639720243849098 ) ) ;
#4009 = PLANE ( 'NONE',  #5875 ) ;
#4011 = ORIENTED_EDGE ( 'NONE', *, *, #1754, .T. ) ;
#4012 = DIRECTION ( 'NONE',  ( 0.000000000000000000, -1.000000000000000000, -1.224646799147350002E-16 ) ) ;
#4013 = CARTESIAN_POINT ( 'NONE',  ( 2.500300139188999182, -51.00737899243799944, 19.50231026484398456 ) ) ;
#4014 = ORIENTED_EDGE ( 'NONE', *, *, #9202, .F. ) ;
#4015 = ORIENTED_EDGE ( 'NONE', *, *, #13272, .T. ) ;
#4016 = CIRCLE ( 'NONE', #12572, 2.499999999999998668 ) ;
#4017 = DIRECTION ( 'NONE',  ( 8.018662683283438208E-16, -5.975035461963189015E-16, -1.000000000000000000 ) ) ;
#4018 = ORIENTED_EDGE ( 'NONE', *, *, #6592, .T. ) ;
#4019 = EDGE_CURVE ( 'NONE', #11184, #9234, #10043, .T. ) ;
#4020 = CARTESIAN_POINT ( 'NONE',  ( -15.49969986081099904, -2.007378992438000331, 24.21206422150100579 ) ) ;
#4021 =( BOUNDED_CURVE ( )  B_SPLINE_CURVE ( 3, ( #11464, #12695, #2061, #839 ),
 .UNSPECIFIED., .F., .T. ) 
 B_SPLINE_CURVE_WITH_KNOTS ( ( 4, 4 ),
 ( 4.712388980384689674, 6.283185307179586232 ),
 .UNSPECIFIED. ) 
 CURVE ( )  GEOMETRIC_REPRESENTATION_ITEM ( )  RATIONAL_B_SPLINE_CURVE ( ( 1.000000000000000000, 0.8047378541243649375, 0.8047378541243649375, 1.000000000000000000 ) ) 
 REPRESENTATION_ITEM ( '' )  );
#4022 = AXIS2_PLACEMENT_3D ( 'NONE', #14110, #422, #3555 ) ;
#4023 = ADVANCED_FACE ( 'NONE', ( #13438 ), #10981, .F. ) ;
#4024 = DIRECTION ( 'NONE',  ( 0.000000000000000000, 0.7071067811865489050, 0.7071067811865462405 ) ) ;
#4025 = DIRECTION ( 'NONE',  ( 8.018662683283438208E-16, -5.975035461963189015E-16, -1.000000000000000000 ) ) ;
#4026 = ADVANCED_FACE ( 'NONE', ( #225 ), #4091, .T. ) ;
#4027 = VECTOR ( 'NONE', #10245, 1000.000000000000114 ) ;
#4028 = CARTESIAN_POINT ( 'NONE',  ( 2.436724872741607317, 11.05255549926114078, 32.21545598377514352 ) ) ;
#4029 = PLANE ( 'NONE',  #9874 ) ;
#4030 = DIRECTION ( 'NONE',  ( 0.000000000000000000, -1.000000000000000000, -1.224646799147350002E-16 ) ) ;
#4031 = ORIENTED_EDGE ( 'NONE', *, *, #1250, .F. ) ;
#4032 = DIRECTION ( 'NONE',  ( 1.000000000000000000, 1.201369187114119994E-15, 9.616040805000176517E-16 ) ) ;
#4033 = CARTESIAN_POINT ( 'NONE',  ( -15.61203582816999891, -107.1622375242508696, -7.140479451889716778 ) ) ;
#4034 = ORIENTED_EDGE ( 'NONE', *, *, #11569, .T. ) ;
#4035 = B_SPLINE_CURVE_WITH_KNOTS ( 'NONE', 3,
 ( #9402, #3513, #12787, #4900, #4742, #6019, #13010, #7087, #1294, #10703, #11619, #14070 ),
 .UNSPECIFIED., .F., .F.,
 ( 4, 2, 2, 2, 2, 4 ),
 ( 0.8546984898013801901, 0.8910238673510351148, 0.9273492449006901506, 0.9455119336755175574, 0.9636746224503449643, 1.000000000000000000 ),
 .UNSPECIFIED. ) ;
#4036 = CARTESIAN_POINT ( 'NONE',  ( 21.92064319118239624, -24.85867307568577544, 26.65960893809553056 ) ) ;
#4037 = ORIENTED_EDGE ( 'NONE', *, *, #2961, .T. ) ;
#4038 = CARTESIAN_POINT ( 'NONE',  ( -7.886584594865190034, -46.96511696614940234, 17.04457229113261718 ) ) ;
#4039 = ORIENTED_EDGE ( 'NONE', *, *, #8298, .F. ) ;
#4040 = DIRECTION ( 'NONE',  ( 0.000000000000000000, 1.000000000000000000, 1.224646799147350002E-16 ) ) ;
#4041 = VECTOR ( 'NONE', #3667, 1000.000000000000000 ) ;
#4042 = DIRECTION ( 'NONE',  ( -1.000000000000000000, 0.000000000000000000, 0.000000000000000000 ) ) ;
#4043 = ADVANCED_FACE ( 'NONE', ( #5385 ), #11922, .F. ) ;
#4044 = LINE ( 'NONE', #1594, #3092 ) ;
#4045 = CARTESIAN_POINT ( 'NONE',  ( -11.90127153857805453, -52.50737899243803497, -13.49768973515603498 ) ) ;
#4046 = CARTESIAN_POINT ( 'NONE',  ( -15.19545581216392627, -5.437764035151672282, 56.85231026484398598 ) ) ;
#4047 = EDGE_LOOP ( 'NONE', ( #13813, #10275, #14082, #4241 ) ) ;
#4048 = CARTESIAN_POINT ( 'NONE',  ( 4.000300139189000959, -20.37340439622242982, -17.99768973515599768 ) ) ;
#4049 = DIRECTION ( 'NONE',  ( 0.5975035461963189576, 0.8018662683283437342, 0.000000000000000000 ) ) ;
#4050 = ORIENTED_EDGE ( 'NONE', *, *, #5771, .F. ) ;
#4052 = ORIENTED_EDGE ( 'NONE', *, *, #14799, .F. ) ;
#4051 = LINE ( 'NONE', #6334, #7636 ) ;
#4053 = ORIENTED_EDGE ( 'NONE', *, *, #4108, .F. ) ;
#4054 = EDGE_CURVE ( 'NONE', #12536, #13190, #13505, .T. ) ;
#4055 = CARTESIAN_POINT ( 'NONE',  ( -11.68798435751175369, -21.74340199640734994, 57.00231026484399166 ) ) ;
#4056 = CARTESIAN_POINT ( 'NONE',  ( -16.17213342976032209, -5.460076146431361188, 57.00231026484397745 ) ) ;
#4057 = AXIS2_PLACEMENT_3D ( 'NONE', #2566, #3712, #7446 ) ;
#4058 = CARTESIAN_POINT ( 'NONE',  ( -11.55178736972959896, -19.37894070656198764, 56.85231026484400019 ) ) ;
#4059 = LINE ( 'NONE', #8494, #2327 ) ;
#4060 = AXIS2_PLACEMENT_3D ( 'NONE', #9226, #7068, #11528 ) ;
#4061 = CARTESIAN_POINT ( 'NONE',  ( -12.37415300023346809, -4.034703455804747207, 56.85231026484398598 ) ) ;
#4062 = CYLINDRICAL_SURFACE ( 'NONE', #3131, 0.2500000000000007216 ) ;
#4063 = LINE ( 'NONE', #11253, #1049 ) ;
#4064 = ORIENTED_EDGE ( 'NONE', *, *, #8490, .T. ) ;
#4065 = LINE ( 'NONE', #8724, #9570 ) ;
#4066 = ORIENTED_EDGE ( 'NONE', *, *, #14180, .T. ) ;
#4068 = ORIENTED_EDGE ( 'NONE', *, *, #14054, .F. ) ;
#4067 = CARTESIAN_POINT ( 'NONE',  ( -7.754798889200088752, -46.50763646577239285, -7.996864293225370623 ) ) ;
#4069 = ORIENTED_EDGE ( 'NONE', *, *, #1842, .F. ) ;
#4070 = EDGE_CURVE ( 'NONE', #15056, #12659, #2009, .T. ) ;
#4071 = DIRECTION ( 'NONE',  ( 0.000000000000000000, -1.000000000000000000, -1.224646799147350002E-16 ) ) ;
#4072 = EDGE_LOOP ( 'NONE', ( #762, #1587 ) ) ;
#4073 = CARTESIAN_POINT ( 'NONE',  ( -15.20204784330336878, -9.007378992438004772, -13.28793577849899599 ) ) ;
#4074 = CARTESIAN_POINT ( 'NONE',  ( -15.53608329785963527, -13.54167542823733328, 56.85231026484398598 ) ) ;
#4075 = DIRECTION ( 'NONE',  ( 5.000000000000000389E-16, -0.4999999999999998890, -0.8660254037844387076 ) ) ;
#4076 = VECTOR ( 'NONE', #9552, 999.9999999999998863 ) ;
#4077 = PRESENTATION_LAYER_ASSIGNMENT (  '', '', ( #7235 ) ) ;
#4079 = CARTESIAN_POINT ( 'NONE',  ( -15.61203582816999891, -107.5495670694337207, -7.066625679870576882 ) ) ;
#4078 = DIRECTION ( 'NONE',  ( 0.000000000000000000, 0.000000000000000000, -1.000000000000000000 ) ) ;
#4080 = ORIENTED_EDGE ( 'NONE', *, *, #15002, .T. ) ;
#4081 = PLANE ( 'NONE',  #10954 ) ;
#4082 = VECTOR ( 'NONE', #2504, 1000.000000000000000 ) ;
#4083 = ORIENTED_EDGE ( 'NONE', *, *, #8093, .F. ) ;
#4084 = CARTESIAN_POINT ( 'NONE',  ( -15.49969986081099904, -57.00737899243800655, -13.49768973515600301 ) ) ;
#4085 = ORIENTED_EDGE ( 'NONE', *, *, #1521, .F. ) ;
#4086 = ORIENTED_EDGE ( 'NONE', *, *, #12377, .F. ) ;
#4087 = EDGE_CURVE ( 'NONE', #8099, #2658, #5162, .T. ) ;
#4088 = CARTESIAN_POINT ( 'NONE',  ( -23.49969986081099904, -44.50737899243799944, -5.497689735156002122 ) ) ;
#4089 = VERTEX_POINT ( 'NONE', #2945 ) ;
#4090 = AXIS2_PLACEMENT_3D ( 'NONE', #14659, #11067, #589 ) ;
#4091 = CYLINDRICAL_SURFACE ( 'NONE', #5672, 0.2499999999999997502 ) ;
#4092 = EDGE_CURVE ( 'NONE', #1165, #1325, #3017, .T. ) ;
#4093 = LINE ( 'NONE', #5317, #13321 ) ;
#4094 = CARTESIAN_POINT ( 'NONE',  ( 9.000300139189000959, -27.00737899243800300, 45.71206422150100224 ) ) ;
#4095 = B_SPLINE_CURVE_WITH_KNOTS ( 'NONE', 3,
 ( #6158, #14131, #8460, #14361, #8612, #8538, #7225, #3724, #9535, #8380 ),
 .UNSPECIFIED., .F., .F.,
 ( 4, 2, 2, 2, 4 ),
 ( 0.2880475688081467478, 0.4353390005973231114, 0.5089847164919113487, 0.5826304323864994750, 0.8772132959648567541 ),
 .UNSPECIFIED. ) ;
#4096 = CARTESIAN_POINT ( 'NONE',  ( 15.30745245775401564, -24.78701188282911261, 2.829765091595426441 ) ) ;
#4097 = CIRCLE ( 'NONE', #9957, 9.974999999999999645 ) ;
#4098 = VECTOR ( 'NONE', #8214, 1000.000000000000114 ) ;
#4099 = LINE ( 'NONE', #1883, #1327 ) ;
#4100 = CARTESIAN_POINT ( 'NONE',  ( -23.55378106252664239, -12.92169478045303066, 56.85231026484398598 ) ) ;
#4101 = AXIS2_PLACEMENT_3D ( 'NONE', #10025, #14855, #6724 ) ;
#4102 = VERTEX_POINT ( 'NONE', #12357 ) ;
#4103 = CARTESIAN_POINT ( 'NONE',  ( -15.57469986081333424, -26.50737899243800300, 57.00223526477140013 ) ) ;
#4104 = CARTESIAN_POINT ( 'NONE',  ( -15.47724068538499154, -13.46270701644446177, 56.85231026484398598 ) ) ;
#4105 = ORIENTED_EDGE ( 'NONE', *, *, #3781, .F. ) ;
#4106 = EDGE_CURVE ( 'NONE', #6628, #5981, #6519, .T. ) ;
#4108 = EDGE_CURVE ( 'NONE', #4618, #8578, #8904, .T. ) ;
#4107 = DIRECTION ( 'NONE',  ( -8.018662683283438208E-16, 5.975035461963189015E-16, 1.000000000000000000 ) ) ;
#4109 =( BOUNDED_CURVE ( )  B_SPLINE_CURVE ( 3, ( #11164, #2976, #687, #6559 ),
 .UNSPECIFIED., .F., .T. ) 
 B_SPLINE_CURVE_WITH_KNOTS ( ( 4, 4 ),
 ( 5.024656459356720006, 6.283185307179586232 ),
 .UNSPECIFIED. ) 
 CURVE ( )  GEOMETRIC_REPRESENTATION_ITEM ( )  RATIONAL_B_SPLINE_CURVE ( ( 1.000000000000000000, 0.8723071003127500500, 0.8723071003127500500, 1.000000000000000000 ) ) 
 REPRESENTATION_ITEM ( '' )  );
#4110 = CARTESIAN_POINT ( 'NONE',  ( -15.49969986081099194, -52.50737899243800655, 11.50231026484399521 ) ) ;
#4111 = ORIENTED_EDGE ( 'NONE', *, *, #10681, .T. ) ;
#4112 = LINE ( 'NONE', #12078, #1032 ) ;
#4113 = EDGE_CURVE ( 'NONE', #7645, #1909, #6591, .T. ) ;
#4114 = VECTOR ( 'NONE', #4746, 1000.000000000000114 ) ;
#4115 = VECTOR ( 'NONE', #4660, 1000.000000000000000 ) ;
#4116 = CARTESIAN_POINT ( 'NONE',  ( -12.66248504435161948, -4.886969368454929352, 56.85231026484398598 ) ) ;
#4117 = EDGE_CURVE ( 'NONE', #13725, #4633, #6371, .T. ) ;
#4118 = DIRECTION ( 'NONE',  ( 0.9755678736739583634, -0.2196982563774038943, 9.135454576426008610E-16 ) ) ;
#4119 =( GEOMETRIC_REPRESENTATION_CONTEXT ( 3 ) GLOBAL_UNCERTAINTY_ASSIGNED_CONTEXT ( ( #8331 ) ) GLOBAL_UNIT_ASSIGNED_CONTEXT ( ( #13863, #3155, #14859 ) ) REPRESENTATION_CONTEXT ( 'NONE', 'WORKASPACE' ) );
#4120 = CYLINDRICAL_SURFACE ( 'NONE', #3807, 0.2000000000000012046 ) ;
#4121 = CARTESIAN_POINT ( 'NONE',  ( -15.49969986081100437, -103.1269401686548690, -4.922466869613988827 ) ) ;
#4122 = EDGE_LOOP ( 'NONE', ( #3525, #8413, #800, #62 ) ) ;
#4123 = CARTESIAN_POINT ( 'NONE',  ( -15.11203582816999891, -107.4899781488447985, -7.806719612820867127 ) ) ;
#4124 = EDGE_CURVE ( 'NONE', #3694, #1385, #6970, .T. ) ;
#4125 = EDGE_CURVE ( 'NONE', #6512, #13055, #3881, .T. ) ;
#4126 = ORIENTED_EDGE ( 'NONE', *, *, #5431, .F. ) ;
#4128 = EDGE_LOOP ( 'NONE', ( #2997, #7767, #13560, #260 ) ) ;
#4127 = LINE ( 'NONE', #8639, #14252 ) ;
#4129 = ORIENTED_EDGE ( 'NONE', *, *, #7549, .F. ) ;
#4130 = CARTESIAN_POINT ( 'NONE',  ( 4.500300139189000959, -19.50737899243801010, -7.509379629622798369 ) ) ;
#4131 = ORIENTED_EDGE ( 'NONE', *, *, #4388, .T. ) ;
#4132 = CIRCLE ( 'NONE', #2909, 0.1500000000000015488 ) ;
#4133 = EDGE_LOOP ( 'NONE', ( #7632, #3269, #2083, #5272, #10715, #5606 ) ) ;
#4134 = CARTESIAN_POINT ( 'NONE',  ( -15.49969986081099904, -57.00737899243800655, 19.50231026484399877 ) ) ;
#4135 = CARTESIAN_POINT ( 'NONE',  ( -14.61203582816999891, -108.1070660607018397, -6.416813587133916030 ) ) ;
#4136 = DIRECTION ( 'NONE',  ( 0.000000000000000000, 0.000000000000000000, 1.000000000000000000 ) ) ;
#4137 = LINE ( 'NONE', #621, #11676 ) ;
#4138 = EDGE_CURVE ( 'NONE', #3941, #6584, #9280, .T. ) ;
#4139 = CARTESIAN_POINT ( 'NONE',  ( -13.11366204365393706, -12.47935976348540876, 51.00231026484399166 ) ) ;
#4140 = AXIS2_PLACEMENT_3D ( 'NONE', #2233, #11565, #5745 ) ;
#4141 = AXIS2_PLACEMENT_3D ( 'NONE', #4952, #9533, #14201 ) ;
#4142 = FACE_OUTER_BOUND ( 'NONE', #10254, .T. ) ;
#4143 = ORIENTED_EDGE ( 'NONE', *, *, #10083, .T. ) ;
#4144 = LINE ( 'NONE', #14549, #1268 ) ;
#4145 = ORIENTED_EDGE ( 'NONE', *, *, #5599, .F. ) ;
#4146 = CARTESIAN_POINT ( 'NONE',  ( -6.726903101582546007, -11.18374239837452500, 56.85231026484400019 ) ) ;
#4148 = ORIENTED_EDGE ( 'NONE', *, *, #388, .F. ) ;
#4147 = CARTESIAN_POINT ( 'NONE',  ( -7.758527451665001351, -44.50737899243799944, -5.497689735156000346 ) ) ;
#4149 = ORIENTED_EDGE ( 'NONE', *, *, #6043, .F. ) ;
#4150 = DIRECTION ( 'NONE',  ( 0.000000000000000000, 1.850371707708594316E-16, -1.000000000000000000 ) ) ;
#4152 = ORIENTED_EDGE ( 'NONE', *, *, #14745, .F. ) ;
#4151 = CARTESIAN_POINT ( 'NONE',  ( -15.49969986081092088, -13.50737899243822504, 57.00231026484397745 ) ) ;
#4153 = CARTESIAN_POINT ( 'NONE',  ( -11.59433051269579806, -11.25225515987115266, -13.08438853397158219 ) ) ;
#4154 = AXIS2_PLACEMENT_3D ( 'NONE', #2106, #6830, #9283 ) ;
#4155 = PLANE ( 'NONE',  #5855 ) ;
#4156 = DIRECTION ( 'NONE',  ( 0.8018662683283436232, -0.5975035461963189576, 9.999999999999998805E-16 ) ) ;
#4157 = EDGE_CURVE ( 'NONE', #4294, #9099, #805, .T. ) ;
#4158 = ADVANCED_FACE ( 'NONE', ( #5460 ), #3471, .F. ) ;
#4159 = AXIS2_PLACEMENT_3D ( 'NONE', #13806, #11505, #1029 ) ;
#4161 = DIRECTION ( 'NONE',  ( -0.4999999999999985012, -0.8660254037844393737, 0.000000000000000000 ) ) ;
#4160 = CARTESIAN_POINT ( 'NONE',  ( -12.60362876103445018, -23.05271278361805543, 54.00231026484399166 ) ) ;
#4162 = ORIENTED_EDGE ( 'NONE', *, *, #8914, .T. ) ;
#4163 = CARTESIAN_POINT ( 'NONE',  ( -11.16775676328318845, -22.49263881059495063, 54.00231026484399166 ) ) ;
#4164 = DIRECTION ( 'NONE',  ( -0.5975035461963172922, -0.8018662683283449555, 0.000000000000000000 ) ) ;
#4165 = ORIENTED_EDGE ( 'NONE', *, *, #2331, .F. ) ;
#4166 = ORIENTED_EDGE ( 'NONE', *, *, #11514, .F. ) ;
#4167 = CARTESIAN_POINT ( 'NONE',  ( -23.52886110248590867, -17.73748770914800943, 56.85231026484398598 ) ) ;
#4168 = ORIENTED_EDGE ( 'NONE', *, *, #723, .T. ) ;
#4169 = CARTESIAN_POINT ( 'NONE',  ( -11.95473997639952302, -37.33086289605605401, 56.83510453573490651 ) ) ;
#4170 = VECTOR ( 'NONE', #2539, 1000.000000000000114 ) ;
#4171 = CARTESIAN_POINT ( 'NONE',  ( 4.878832129573360987, 5.990273379225493855, 18.87332414979169570 ) ) ;
#4172 = FACE_OUTER_BOUND ( 'NONE', #4379, .T. ) ;
#4173 = ADVANCED_FACE ( 'NONE', ( #13878 ), #8113, .T. ) ;
#4174 = CARTESIAN_POINT ( 'NONE',  ( 17.02395575395021154, -23.74935330727123173, 5.539182377213959008 ) ) ;
#4175 = CARTESIAN_POINT ( 'NONE',  ( -15.49969986081092088, -13.50737899243822504, 57.00231026484397745 ) ) ;
#4176 = DIRECTION ( 'NONE',  ( -9.702032863404950344E-16, 1.000000000000000000, 0.000000000000000000 ) ) ;
#4177 = ORIENTED_EDGE ( 'NONE', *, *, #531, .T. ) ;
#4178 = CARTESIAN_POINT ( 'NONE',  ( -15.49969986081099904, 22.99262100756200056, 24.21206422150100224 ) ) ;
#4179 = CARTESIAN_POINT ( 'NONE',  ( 22.00030013918900096, -27.00737899243800300, 46.46206422150100224 ) ) ;
#4180 = EDGE_LOOP ( 'NONE', ( #10941, #10905, #10554, #4080, #9864, #3264 ) ) ;
#4181 = CARTESIAN_POINT ( 'NONE',  ( 2.304527317575351564, 7.441414002149848272, 30.84924175176620764 ) ) ;
#4182 = CARTESIAN_POINT ( 'NONE',  ( 21.99845600427570247, -23.77846206701320142, 23.78571393264229883 ) ) ;
#4183 = CARTESIAN_POINT ( 'NONE',  ( -23.96284084890188382, -10.23071992935364527, 57.00231026484397745 ) ) ;
#4184 = VERTEX_POINT ( 'NONE', #2251 ) ;
#4185 = CARTESIAN_POINT ( 'NONE',  ( -15.49969986081092088, -13.50737899243822504, 57.00231026484397745 ) ) ;
#4186 = AXIS2_PLACEMENT_3D ( 'NONE', #10551, #2010, #8961 ) ;
#4187 = DIRECTION ( 'NONE',  ( -0.4895147004624045839, 0.8719950447285823580, -9.135454576426008610E-16 ) ) ;
#4188 = B_SPLINE_CURVE_WITH_KNOTS ( 'NONE', 3,
 ( #6473, #6552, #14601, #11005, #13319, #12309, #1828, #6329, #13609, #11157, #7777, #11237 ),
 .UNSPECIFIED., .F., .F.,
 ( 4, 2, 2, 2, 2, 4 ),
 ( 0.000000000000000000, 0.2499999999999938938, 0.3749999999999918399, 0.4374999999999926725, 0.4999999999999935607, 1.000000000000000000 ),
 .UNSPECIFIED. ) ;
#4189 = APPLICATION_PROTOCOL_DEFINITION ( 'draft international standard', 'automotive_design', 1998, #9478 ) ;
#4190 = EDGE_CURVE ( 'NONE', #12810, #6704, #5684, .T. ) ;
#4191 = CARTESIAN_POINT ( 'NONE',  ( -7.660032944547833011, -48.43376236753700681, 21.09577438474947186 ) ) ;
#4192 = FACE_OUTER_BOUND ( 'NONE', #5641, .T. ) ;
#4193 = CARTESIAN_POINT ( 'NONE',  ( -14.07534335717186202, -5.558639560896826204, 56.85231026484398598 ) ) ;
#4194 = EDGE_CURVE ( 'NONE', #13942, #12795, #12588, .T. ) ;
#4195 = ORIENTED_EDGE ( 'NONE', *, *, #5778, .T. ) ;
#4196 = CARTESIAN_POINT ( 'NONE',  ( -12.60362876103445373, -23.05271278361805543, 57.00231026484399166 ) ) ;
#4197 =( BOUNDED_CURVE ( )  B_SPLINE_CURVE ( 3, ( #7725, #3380, #12568, #12410 ),
 .UNSPECIFIED., .F., .F. ) 
 B_SPLINE_CURVE_WITH_KNOTS ( ( 4, 4 ),
 ( 5.060245233341797544, 5.259239931080632147 ),
 .UNSPECIFIED. ) 
 CURVE ( )  GEOMETRIC_REPRESENTATION_ITEM ( )  RATIONAL_B_SPLINE_CURVE ( ( 1.000000000000000000, 0.9967028139718016044, 0.9967028139718016044, 1.000000000000000000 ) ) 
 REPRESENTATION_ITEM ( '' )  );
#4198 = CARTESIAN_POINT ( 'NONE',  ( -15.49969986081091733, -13.50737899243822682, 54.00231026484399166 ) ) ;
#4199 = VECTOR ( 'NONE', #10404, 1000.000000000000000 ) ;
#4200 = ORIENTED_EDGE ( 'NONE', *, *, #5064, .T. ) ;
#4202 = VERTEX_POINT ( 'NONE', #4399 ) ;
#4201 = FACE_OUTER_BOUND ( 'NONE', #12347, .T. ) ;
#4203 = EDGE_CURVE ( 'NONE', #7811, #1260, #7221, .T. ) ;
#4204 = ORIENTED_EDGE ( 'NONE', *, *, #7924, .T. ) ;
#4205 = DIRECTION ( 'NONE',  ( 1.000000000000000000, -3.922012711866029438E-32, 3.202566417187950042E-16 ) ) ;
#4206 = FACE_OUTER_BOUND ( 'NONE', #13027, .T. ) ;
#4207 = AXIS2_PLACEMENT_3D ( 'NONE', #14258, #5984, #7046 ) ;
#4208 = FACE_OUTER_BOUND ( 'NONE', #5751, .T. ) ;
#4209 = CARTESIAN_POINT ( 'NONE',  ( -8.660471612933879015, -48.65904406005358851, 45.78551480191092793 ) ) ;
#4210 = AXIS2_PLACEMENT_3D ( 'NONE', #1682, #5201, #6410 ) ;
#4211 = AXIS2_PLACEMENT_3D ( 'NONE', #10351, #15018, #3396 ) ;
#4212 = AXIS2_PLACEMENT_3D ( 'NONE', #8321, #3813, #12006 ) ;
#4213 = ADVANCED_FACE ( 'NONE', ( #8049 ), #5610, .F. ) ;
#4214 = DIRECTION ( 'NONE',  ( -0.8934395198752397294, 0.4491835085186243748, -9.848077530122081084E-16 ) ) ;
#4215 = EDGE_CURVE ( 'NONE', #858, #6590, #12663, .T. ) ;
#4216 = CYLINDRICAL_SURFACE ( 'NONE', #8941, 2.999999999999999112 ) ;
#4217 = FACE_OUTER_BOUND ( 'NONE', #398, .T. ) ;
#4218 = CARTESIAN_POINT ( 'NONE',  ( -16.32149003149046607, -5.473954385499126829, 56.85231026484398598 ) ) ;
#4219 = ORIENTED_EDGE ( 'NONE', *, *, #9952, .F. ) ;
#4220 = CARTESIAN_POINT ( 'NONE',  ( -21.29301345516119071, -7.881655252552254964, 57.00231026484397745 ) ) ;
#4221 = ORIENTED_EDGE ( 'NONE', *, *, #4113, .F. ) ;
#4222 = DIRECTION ( 'NONE',  ( 0.000000000000000000, 0.000000000000000000, -1.000000000000000000 ) ) ;
#4223 = EDGE_LOOP ( 'NONE', ( #14389, #6366 ) ) ;
#4224 = ORIENTED_EDGE ( 'NONE', *, *, #13794, .F. ) ;
#4225 = DIRECTION ( 'NONE',  ( -8.018662683283438208E-16, 5.975035461963189015E-16, 1.000000000000000000 ) ) ;
#4226 = CIRCLE ( 'NONE', #11549, 15.62500000000000355 ) ;
#4227 = DIRECTION ( 'NONE',  ( -1.000000000000000078E-15, 1.000000000000000000, 0.000000000000000000 ) ) ;
#4229 = ORIENTED_EDGE ( 'NONE', *, *, #11629, .T. ) ;
#4228 = CARTESIAN_POINT ( 'NONE',  ( 1.973171000691426702, 8.982922429311637202, 16.74883253750077117 ) ) ;
#4230 = CARTESIAN_POINT ( 'NONE',  ( -15.49969986081091022, -13.50737899243823215, 46.00231026484398456 ) ) ;
#4231 = DIRECTION ( 'NONE',  ( 0.8599296884906633132, -0.5104125104778985955, 9.945218953682734920E-16 ) ) ;
#4232 = EDGE_CURVE ( 'NONE', #10290, #2754, #14094, .T. ) ;
#4233 = VECTOR ( 'NONE', #14774, 1000.000000000000227 ) ;
#4234 = EDGE_CURVE ( 'NONE', #3406, #4445, #6128, .T. ) ;
#4235 = FACE_OUTER_BOUND ( 'NONE', #12165, .T. ) ;
#4236 = CARTESIAN_POINT ( 'NONE',  ( -15.49969986081092088, -13.50737899243822504, 57.00231026484397745 ) ) ;
#4237 = ORIENTED_EDGE ( 'NONE', *, *, #788, .F. ) ;
#4238 = DIRECTION ( 'NONE',  ( 8.018662683283438208E-16, -5.975035461963189015E-16, -1.000000000000000000 ) ) ;
#4239 = CYLINDRICAL_SURFACE ( 'NONE', #11409, 5.000000000000000000 ) ;
#4240 = ORIENTED_EDGE ( 'NONE', *, *, #4296, .F. ) ;
#4241 = ORIENTED_EDGE ( 'NONE', *, *, #10600, .T. ) ;
#4242 = CARTESIAN_POINT ( 'NONE',  ( -15.49969986081099194, -27.00737899243800300, 11.50231026484399877 ) ) ;
#4243 = ORIENTED_EDGE ( 'NONE', *, *, #3986, .F. ) ;
#4245 = EDGE_CURVE ( 'NONE', #2060, #2729, #11302, .T. ) ;
#4244 = DIRECTION ( 'NONE',  ( 0.000000000000000000, 1.272130549049658454E-16, -1.000000000000000000 ) ) ;
#4246 = AXIS2_PLACEMENT_3D ( 'NONE', #6629, #6705, #14830 ) ;
#4247 = DIRECTION ( 'NONE',  ( -9.912705577010322591E-16, 0.1872998510044552312, 0.9823027872370662106 ) ) ;
#4248 = DIRECTION ( 'NONE',  ( 0.000000000000000000, 0.000000000000000000, 1.000000000000000000 ) ) ;
#4249 = VECTOR ( 'NONE', #8593, 1000.000000000000000 ) ;
#4250 = CARTESIAN_POINT ( 'NONE',  ( -31.79969986081099975, 20.99262100756200056, 32.26206422150099939 ) ) ;
#4251 = VECTOR ( 'NONE', #9297, 1000.000000000000000 ) ;
#4252 = DIRECTION ( 'NONE',  ( -0.5779813897169902015, 0.8160499452489514693, -9.510565162951533652E-16 ) ) ;
#4254 = DIRECTION ( 'NONE',  ( -1.054621095516909827E-16, 0.000000000000000000, 1.000000000000000000 ) ) ;
#4253 = DIRECTION ( 'NONE',  ( -8.018662683283438208E-16, 5.975035461963189015E-16, 1.000000000000000000 ) ) ;
#4255 = VERTEX_POINT ( 'NONE', #1332 ) ;
#4256 = DIRECTION ( 'NONE',  ( 0.000000000000000000, 0.1872998510044759646, 0.9823027872370621028 ) ) ;
#4257 = CARTESIAN_POINT ( 'NONE',  ( -15.49969986081099016, -110.5850680553859746, -10.73408862071934067 ) ) ;
#4258 = EDGE_LOOP ( 'NONE', ( #4652, #11623, #3316, #5239 ) ) ;
#4259 = PLANE ( 'NONE',  #12025 ) ;
#4260 = FACE_BOUND ( 'NONE', #5550, .T. ) ;
#4261 = CIRCLE ( 'NONE', #12084, 5.000000000000000000 ) ;
#4262 = ORIENTED_EDGE ( 'NONE', *, *, #3311, .T. ) ;
#4263 = FACE_OUTER_BOUND ( 'NONE', #13074, .T. ) ;
#4264 = ADVANCED_FACE ( 'NONE', ( #7204 ), #4856, .F. ) ;
#4265 = CIRCLE ( 'NONE', #12825, 1.300000000000000488 ) ;
#4266 = PLANE ( 'NONE',  #1762 ) ;
#4267 = APPLICATION_PROTOCOL_DEFINITION ( 'draft international standard', 'automotive_design', 1998, #4297 ) ;
#4268 = PLANE ( 'NONE',  #2370 ) ;
#4269 = CARTESIAN_POINT ( 'NONE',  ( -16.34789837066772122, -3.568506607309356315, 56.85231026484398598 ) ) ;
#4270 = CARTESIAN_POINT ( 'NONE',  ( -18.09969986081100046, -107.1622034095870077, -6.087689735156001980 ) ) ;
#4271 = ORIENTED_EDGE ( 'NONE', *, *, #6544, .T. ) ;
#4272 = DIRECTION ( 'NONE',  ( -1.000000000000000078E-15, 1.000000000000000000, 0.000000000000000000 ) ) ;
#4273 = FACE_OUTER_BOUND ( 'NONE', #8486, .T. ) ;
#4274 = VECTOR ( 'NONE', #1290, 1000.000000000000000 ) ;
#4275 = VERTEX_POINT ( 'NONE', #11885 ) ;
#4277 = VERTEX_POINT ( 'NONE', #10737 ) ;
#4276 = CARTESIAN_POINT ( 'NONE',  ( -1.508527451664999575, -46.50737899243799234, -5.497689735156000346 ) ) ;
#4278 = ORIENTED_EDGE ( 'NONE', *, *, #193, .T. ) ;
#4279 = EDGE_CURVE ( 'NONE', #7908, #4983, #1405, .T. ) ;
#4280 = CARTESIAN_POINT ( 'NONE',  ( -21.11416342254291934, -20.63752968607602867, 56.85231026484398598 ) ) ;
#4281 = CARTESIAN_POINT ( 'NONE',  ( -8.010324353647195750, -47.33175634226493855, 56.24696452326014651 ) ) ;
#4282 = ADVANCED_FACE ( 'NONE', ( #2629 ), #9509, .F. ) ;
#4283 = DIRECTION ( 'NONE',  ( -8.018662683283438208E-16, 5.975035461963189015E-16, 1.000000000000000000 ) ) ;
#4284 = CARTESIAN_POINT ( 'NONE',  ( -14.26755283655060680, -21.48817241857114269, 56.85231026484400019 ) ) ;
#4285 = DIRECTION ( 'NONE',  ( 0.6061090314442014737, -0.7953815700667020705, 9.612616959383187437E-16 ) ) ;
#4286 =( BOUNDED_CURVE ( )  B_SPLINE_CURVE ( 3, ( #5782, #4570, #3276, #5852 ),
 .UNSPECIFIED., .F., .F. ) 
 B_SPLINE_CURVE_WITH_KNOTS ( ( 4, 4 ),
 ( 5.038118467679318258, 5.213043692789276484 ),
 .UNSPECIFIED. ) 
 CURVE ( )  GEOMETRIC_REPRESENTATION_ITEM ( )  RATIONAL_B_SPLINE_CURVE ( ( 1.000000000000000000, 0.9974517222217440526, 0.9974517222217440526, 1.000000000000000000 ) ) 
 REPRESENTATION_ITEM ( '' )  );
#4287 = CARTESIAN_POINT ( 'NONE',  ( -15.57469986081333424, -23.50709773848279482, 57.00223526477140013 ) ) ;
#4288 = LINE ( 'NONE', #11325, #13548 ) ;
#4289 = PLANE ( 'NONE',  #5927 ) ;
#4290 = DIRECTION ( 'NONE',  ( 0.1617534816134024167, -0.9868311969055004740, 7.193398003386505973E-16 ) ) ;
#4291 = ORIENTED_EDGE ( 'NONE', *, *, #5624, .F. ) ;
#4292 = FACE_OUTER_BOUND ( 'NONE', #5020, .T. ) ;
#4294 = VERTEX_POINT ( 'NONE', #13199 ) ;
#4293 = CARTESIAN_POINT ( 'NONE',  ( -18.15085299098534222, -14.64962258016358554, 51.00231026484399166 ) ) ;
#4295 = ORIENTED_EDGE ( 'NONE', *, *, #1488, .T. ) ;
#4296 = EDGE_CURVE ( 'NONE', #12810, #14910, #6965, .T. ) ;
#4297 = APPLICATION_CONTEXT ( 'automotive_design' ) ;
#4298 = FACE_OUTER_BOUND ( 'NONE', #12096, .T. ) ;
#4299 = ADVANCED_FACE ( 'NONE', ( #8204 ), #8513, .F. ) ;
#4301 = ORIENTED_EDGE ( 'NONE', *, *, #12681, .T. ) ;
#4300 = CARTESIAN_POINT ( 'NONE',  ( -15.49969986081099904, 10.68321993080349586, 43.21206422150100224 ) ) ;
#4302 = VECTOR ( 'NONE', #1669, 1000.000000000000000 ) ;
#4303 = DIRECTION ( 'NONE',  ( 0.000000000000000000, -1.000000000000000000, -1.224646799147350002E-16 ) ) ;
#4304 = ADVANCED_FACE ( 'NONE', ( #10583 ), #7125, .F. ) ;
#4305 = CARTESIAN_POINT ( 'NONE',  ( -18.50396719079564889, -6.011671700261853601, 56.85231026484398598 ) ) ;
#4306 = EDGE_CURVE ( 'NONE', #4377, #13245, #5923, .T. ) ;
#4307 = DIRECTION ( 'NONE',  ( -8.018662683283438208E-16, 5.975035461963189015E-16, 1.000000000000000000 ) ) ;
#4308 = VECTOR ( 'NONE', #2749, 1000.000000000000000 ) ;
#4309 = LINE ( 'NONE', #5524, #11058 ) ;
#4310 = ORIENTED_EDGE ( 'NONE', *, *, #3652, .F. ) ;
#4311 = LINE ( 'NONE', #5601, #12162 ) ;
#4312 = ORIENTED_EDGE ( 'NONE', *, *, #2030, .F. ) ;
#4313 = DIRECTION ( 'NONE',  ( -0.8415927028326188886, 0.5401126942952620968, -9.975640502598240034E-16 ) ) ;
#4314 = ORIENTED_EDGE ( 'NONE', *, *, #10377, .T. ) ;
#4315 = VERTEX_POINT ( 'NONE', #3702 ) ;
#4316 = PLANE ( 'NONE',  #6385 ) ;
#4317 = EDGE_CURVE ( 'NONE', #2532, #8254, #4778, .T. ) ;
#4318 = EDGE_CURVE ( 'NONE', #12566, #11022, #12047, .T. ) ;
#4319 = ORIENTED_EDGE ( 'NONE', *, *, #10640, .F. ) ;
#4320 = CARTESIAN_POINT ( 'NONE',  ( -7.757642952717569429, -42.42537882359017942, 56.19456526637834770 ) ) ;
#4321 = AXIS2_PLACEMENT_3D ( 'NONE', #768, #13697, #3137 ) ;
#4322 = FACE_OUTER_BOUND ( 'NONE', #4674, .T. ) ;
#4323 = DIRECTION ( 'NONE',  ( 1.000000000000000000, 1.201369187114119994E-15, 9.616040805000176517E-16 ) ) ;
#4324 = VECTOR ( 'NONE', #7964, 1000.000000000000227 ) ;
#4325 = DIRECTION ( 'NONE',  ( 0.5691548339926102429, 0.8222303661035903488, -3.489949670250048422E-17 ) ) ;
#4326 = UNCERTAINTY_MEASURE_WITH_UNIT (LENGTH_MEASURE( 1.000000000000000082E-05 ), #4858, 'distance_accuracy_value', 'NONE');
#4327 = CIRCLE ( 'NONE', #6749, 9.974999999999999645 ) ;
#4328 = EDGE_CURVE ( 'NONE', #4893, #6007, #14104, .T. ) ;
#4329 = CARTESIAN_POINT ( 'NONE',  ( -7.528759897616733809, -14.80173833325270571, 56.85231026484400019 ) ) ;
#4331 = CARTESIAN_POINT ( 'NONE',  ( 4.913689842097131333, 5.973563155936592040, 29.53187956306727457 ) ) ;
#4330 = DIRECTION ( 'NONE',  ( -1.000000000000000000, 1.927249326158850112E-15, -7.070501591499349439E-17 ) ) ;
#4332 = ORIENTED_EDGE ( 'NONE', *, *, #8990, .F. ) ;
#4333 = CARTESIAN_POINT ( 'NONE',  ( -5.500669204425239656, -13.50739036851649466, 60.35526053768147392 ) ) ;
#4334 = CIRCLE ( 'NONE', #10183, 1.075000000000000400 ) ;
#4335 = DIRECTION ( 'NONE',  ( -8.018662683283438208E-16, 5.975035461963189015E-16, 1.000000000000000000 ) ) ;
#4336 = ORIENTED_EDGE ( 'NONE', *, *, #12759, .T. ) ;
#4337 = ORIENTED_EDGE ( 'NONE', *, *, #13527, .T. ) ;
#4338 = DIRECTION ( 'NONE',  ( 0.9957106782009873536, 0.09252159378507134047, 7.431448254773946593E-16 ) ) ;
#4339 = DIRECTION ( 'NONE',  ( 0.5975035461963189576, 0.8018662683283437342, 0.000000000000000000 ) ) ;
#4340 = DIRECTION ( 'NONE',  ( 0.000000000000000000, -1.000000000000000000, -1.224646799147350002E-16 ) ) ;
#4341 = CARTESIAN_POINT ( 'NONE',  ( -14.84437367148764686, -93.78075803281299727, -10.82899037021154953 ) ) ;
#4342 = VERTEX_POINT ( 'NONE', #3623 ) ;
#4343 = CONICAL_SURFACE ( 'NONE', #12896, 23.00000000000000000, 1.047197551196598297 ) ;
#4344 = LINE ( 'NONE', #5403, #12743 ) ;
#4345 = CARTESIAN_POINT ( 'NONE',  ( 7.000300139189000070, -32.00737899243799944, 54.21206422150100224 ) ) ;
#4346 = CIRCLE ( 'NONE', #11674, 9.974999999999999645 ) ;
#4347 = PRODUCT_CONTEXT ( 'NONE', #13971, 'mechanical' ) ;
#4348 = FACE_OUTER_BOUND ( 'NONE', #6350, .T. ) ;
#4349 = AXIS2_PLACEMENT_3D ( 'NONE', #11710, #13935, #2534 ) ;
#4350 = ADVANCED_FACE ( 'NONE', ( #14261 ), #14337, .F. ) ;
#4351 = PLANE ( 'NONE',  #9917 ) ;
#4352 = CARTESIAN_POINT ( 'NONE',  ( -25.21423696146293736, -11.24278324042065869, 56.85231026484398598 ) ) ;
#4353 = EDGE_LOOP ( 'NONE', ( #8213, #1672, #7039, #389 ) ) ;
#4354 = DIRECTION ( 'NONE',  ( -1.000000000000000000, 0.000000000000000000, 0.000000000000000000 ) ) ;
#4355 = DIRECTION ( 'NONE',  ( -0.5975035461963188466, -0.8018662683283437342, 0.000000000000000000 ) ) ;
#4356 = LINE ( 'NONE', #12540, #14756 ) ;
#4357 = VERTEX_POINT ( 'NONE', #13047 ) ;
#4359 = VERTEX_POINT ( 'NONE', #1175 ) ;
#4358 = CARTESIAN_POINT ( 'NONE',  ( 14.68618260102869932, -27.00737899243800300, 46.46206422150099513 ) ) ;
#4360 = B_SPLINE_CURVE_WITH_KNOTS ( 'NONE', 3,
 ( #3392, #8042, #6118, #13112, #12964, #2322, #9503, #1324, #9272, #12882, #14097, #1473, #15088, #5825, #13943, #109, #8118, #11644 ),
 .UNSPECIFIED., .F., .F.,
 ( 4, 2, 2, 2, 2, 2, 2, 2, 4 ),
 ( 0.01418968994342788455, 0.01507654967364544137, 0.01596340940386299992, 0.01685026913408055674, 0.01773712886429811356, 0.01862398859451567384, 0.01951084832473323066, 0.02039770805495078748, 0.02128456778516834430 ),
 .UNSPECIFIED. ) ;
#4361 = ORIENTED_EDGE ( 'NONE', *, *, #12913, .T. ) ;
#4362 = CARTESIAN_POINT ( 'NONE',  ( -8.663330333365388825, -17.80566954616001496, 56.85231026484400019 ) ) ;
#4363 = DIRECTION ( 'NONE',  ( -1.000000000000000000, 0.000000000000000000, 0.000000000000000000 ) ) ;
#4364 = LINE ( 'NONE', #3134, #4708 ) ;
#4365 = CARTESIAN_POINT ( 'NONE',  ( -21.21771647519868154, -9.340181373223902739, 56.85231026484398598 ) ) ;
#4366 = VECTOR ( 'NONE', #8585, 1000.000000000000000 ) ;
#4367 = CARTESIAN_POINT ( 'NONE',  ( -18.36422177163696290, -5.957162821864243618, 56.85231026484398598 ) ) ;
#4368 = ADVANCED_FACE ( 'NONE', ( #5832 ), #1703, .T. ) ;
#4369 = CARTESIAN_POINT ( 'NONE',  ( -19.05456510292772876, -4.187316862259577555, 56.85231026484398598 ) ) ;
#4370 = PLANE ( 'NONE',  #366 ) ;
#4371 = CARTESIAN_POINT ( 'NONE',  ( -13.88982576282654691, -4.575998618238553917, 57.00231026484397745 ) ) ;
#4372 = VERTEX_POINT ( 'NONE', #6356 ) ;
#4373 = CARTESIAN_POINT ( 'NONE',  ( 15.21157213869945934, -29.07137141679140768, 45.73161216243208571 ) ) ;
#4374 = ORIENTED_EDGE ( 'NONE', *, *, #8588, .T. ) ;
#4375 = DIRECTION ( 'NONE',  ( 0.9316361277244821215, 0.3633925226508276651, 5.299192642332029177E-16 ) ) ;
#4377 = VERTEX_POINT ( 'NONE', #12113 ) ;
#4376 = CARTESIAN_POINT ( 'NONE',  ( -18.15085299098534222, -14.64962258016358376, 51.25231026484399166 ) ) ;
#4378 = CARTESIAN_POINT ( 'NONE',  ( -9.299228256956212135, -8.333850033420862502, 57.00231026484397745 ) ) ;
#4379 = EDGE_LOOP ( 'NONE', ( #2311, #553, #4544, #14432 ) ) ;
#4380 = LINE ( 'NONE', #2007, #9530 ) ;
#4381 = CARTESIAN_POINT ( 'NONE',  ( 0.000000000000000000, 0.000000000000000000, 0.000000000000000000 ) ) ;
#4382 = CIRCLE ( 'NONE', #3651, 8.314203600725839749 ) ;
#4383 = VECTOR ( 'NONE', #2198, 1000.000000000000000 ) ;
#4384 = EDGE_CURVE ( 'NONE', #12656, #15034, #8616, .T. ) ;
#4385 = EDGE_LOOP ( 'NONE', ( #12143, #3120, #13265, #2627 ) ) ;
#4386 = CARTESIAN_POINT ( 'NONE',  ( -7.886584594865190034, -46.96511696614950182, -7.955427708867500058 ) ) ;
#4387 = FACE_OUTER_BOUND ( 'NONE', #8436, .T. ) ;
#4388 = EDGE_CURVE ( 'NONE', #12952, #12465, #12475, .T. ) ;
#4389 = ORIENTED_EDGE ( 'NONE', *, *, #3115, .T. ) ;
#4390 = CARTESIAN_POINT ( 'NONE',  ( 17.56713017795110332, -24.02660615158903923, 41.90057110130022977 ) ) ;
#4391 = ORIENTED_EDGE ( 'NONE', *, *, #14773, .F. ) ;
#4392 = DIRECTION ( 'NONE',  ( -0.1165201156931293391, -0.9931883319083343320, 4.999999999999997430E-16 ) ) ;
#4393 = ORIENTED_EDGE ( 'NONE', *, *, #8810, .F. ) ;
#4394 = ORIENTED_EDGE ( 'NONE', *, *, #12628, .T. ) ;
#4395 = DIRECTION ( 'NONE',  ( 0.2872152572324145892, 0.9578660637129379207, -3.420201433256678811E-16 ) ) ;
#4396 = VERTEX_POINT ( 'NONE', #6286 ) ;
#4397 = EDGE_CURVE ( 'NONE', #1781, #2885, #9956, .T. ) ;
#4398 = CIRCLE ( 'NONE', #2685, 1.249999999999999778 ) ;
#4399 = CARTESIAN_POINT ( 'NONE',  ( -17.62015867087677634, -21.29935591968936137, 57.00231026484399166 ) ) ;
#4400 = DIRECTION ( 'NONE',  ( -8.018662683283439195E-16, 5.975035461963190001E-16, 1.000000000000000000 ) ) ;
#4401 = CARTESIAN_POINT ( 'NONE',  ( -10.13128693740209840, -90.53913777082694025, -5.691719241778902649 ) ) ;
#4402 = EDGE_CURVE ( 'NONE', #5287, #11156, #13344, .T. ) ;
#4403 = CARTESIAN_POINT ( 'NONE',  ( 14.68618260102867090, -26.77784494758310530, 1.962064221501000683 ) ) ;
#4404 = EDGE_CURVE ( 'NONE', #12600, #10731, #14631, .T. ) ;
#4405 = FACE_OUTER_BOUND ( 'NONE', #1264, .T. ) ;
#4407 = CARTESIAN_POINT ( 'NONE',  ( 4.939584056586554084, 5.961151497827415824, 29.51773124056278164 ) ) ;
#4406 = PLANE ( 'NONE',  #11563 ) ;
#4408 = ORIENTED_EDGE ( 'NONE', *, *, #5821, .F. ) ;
#4409 = DIRECTION ( 'NONE',  ( 0.6859287159822015090, -0.7276687409742212953, 9.848077530122081084E-16 ) ) ;
#4410 = DIRECTION ( 'NONE',  ( 0.000000000000000000, -1.000000000000000000, -1.224646799147350002E-16 ) ) ;
#4411 = ORIENTED_EDGE ( 'NONE', *, *, #5430, .T. ) ;
#4412 = ORIENTED_EDGE ( 'NONE', *, *, #1632, .F. ) ;
#4413 = CARTESIAN_POINT ( 'NONE',  ( -23.49969986081099904, -19.50737899243800300, 56.13904046828879757 ) ) ;
#4414 = AXIS2_PLACEMENT_3D ( 'NONE', #14482, #4231, #12190 ) ;
#4415 = CARTESIAN_POINT ( 'NONE',  ( -18.32592690080561937, -37.01861151523911531, -17.89183167732498347 ) ) ;
#4416 = CARTESIAN_POINT ( 'NONE',  ( -7.734307812155741146, -7.246443652516329159, 54.00231026484399166 ) ) ;
#4417 = FACE_OUTER_BOUND ( 'NONE', #2511, .T. ) ;
#4418 = VERTEX_POINT ( 'NONE', #13418 ) ;
#4419 = DIRECTION ( 'NONE',  ( -0.9320450512859425052, -0.3618458327180908984, 0.01896353653557666941 ) ) ;
#4420 = DIRECTION ( 'NONE',  ( 0.000000000000000000, 0.000000000000000000, 1.000000000000000000 ) ) ;
#4421 = CYLINDRICAL_SURFACE ( 'NONE', #10168, 0.4500000000000011768 ) ;
#4422 = EDGE_CURVE ( 'NONE', #15033, #5603, #3408, .T. ) ;
#4423 =( BOUNDED_CURVE ( )  B_SPLINE_CURVE ( 3, ( #10075, #8854, #1979, #11083 ),
 .UNSPECIFIED., .F., .T. ) 
 B_SPLINE_CURVE_WITH_KNOTS ( ( 4, 4 ),
 ( 5.266983419591681148, 6.776859123585839306 ),
 .UNSPECIFIED. ) 
 CURVE ( )  GEOMETRIC_REPRESENTATION_ITEM ( )  RATIONAL_B_SPLINE_CURVE ( ( 1.000000000000000000, 0.8188760873989417988, 0.8188760873989417988, 1.000000000000000000 ) ) 
 REPRESENTATION_ITEM ( '' )  );
#4424 = DIRECTION ( 'NONE',  ( 0.000000000000000000, 0.1872998510044759646, 0.9823027872370621028 ) ) ;
#4425 = LINE ( 'NONE', #6620, #2315 ) ;
#4426 = ORIENTED_EDGE ( 'NONE', *, *, #7190, .T. ) ;
#4427 = LINE ( 'NONE', #6084, #6029 ) ;
#4428 = CARTESIAN_POINT ( 'NONE',  ( -14.61203582817000068, -108.0739289917894865, -5.561265332623593238 ) ) ;
#4429 = ORIENTED_EDGE ( 'NONE', *, *, #7290, .F. ) ;
#4430 = DIRECTION ( 'NONE',  ( 0.000000000000000000, 1.000000000000000000, 1.224646799147350002E-16 ) ) ;
#4431 = ORIENTED_EDGE ( 'NONE', *, *, #10567, .T. ) ;
#4432 = AXIS2_PLACEMENT_3D ( 'NONE', #13675, #8922, #13601 ) ;
#4433 = CARTESIAN_POINT ( 'NONE',  ( -20.64795620320353109, -18.36032465801230273, 57.00231026484397745 ) ) ;
#4434 = FACE_OUTER_BOUND ( 'NONE', #838, .T. ) ;
#4435 = ADVANCED_FACE ( 'NONE', ( #8809 ), #8732, .T. ) ;
#4436 = DIRECTION ( 'NONE',  ( -0.9731439732146149879, -0.2301973227387160703, -6.427876096865396850E-16 ) ) ;
#4437 = DIRECTION ( 'NONE',  ( 1.000000000000000078E-15, -1.000000000000000000, 0.000000000000000000 ) ) ;
#4438 = CARTESIAN_POINT ( 'NONE',  ( -5.500669204425239656, -13.50739036851649466, 60.35526053768147392 ) ) ;
#4439 = CIRCLE ( 'NONE', #13723, 9.974999999999999645 ) ;
#4440 = CARTESIAN_POINT ( 'NONE',  ( -15.83606446161809167, -16.37446674635458521, 51.25231026484399166 ) ) ;
#4441 = CARTESIAN_POINT ( 'NONE',  ( 0.8003001391889992266, 3.992621007561997892, 24.16206422150099442 ) ) ;
#4442 = LINE ( 'NONE', #8092, #3253 ) ;
#4443 = ORIENTED_EDGE ( 'NONE', *, *, #14931, .F. ) ;
#4444 = CARTESIAN_POINT ( 'NONE',  ( 15.96229431146955058, -29.94371705786681304, 44.61892371905074128 ) ) ;
#4445 = VERTEX_POINT ( 'NONE', #14481 ) ;
#4446 = CYLINDRICAL_SURFACE ( 'NONE', #3095, 0.4500000000000011768 ) ;
#4448 = VERTEX_POINT ( 'NONE', #12339 ) ;
#4447 = CARTESIAN_POINT ( 'NONE',  ( -5.524802968312267026, -13.55273297815671008, 56.85231026484400019 ) ) ;
#4449 = ORIENTED_EDGE ( 'NONE', *, *, #4988, .F. ) ;
#4450 = AXIS2_PLACEMENT_3D ( 'NONE', #12282, #14722, #13356 ) ;
#4451 = ORIENTED_EDGE ( 'NONE', *, *, #4157, .T. ) ;
#4452 = CIRCLE ( 'NONE', #11298, 0.2000000000000012046 ) ;
#4453 = DIRECTION ( 'NONE',  ( 0.000000000000000000, 0.000000000000000000, -1.000000000000000000 ) ) ;
#4454 = EDGE_CURVE ( 'NONE', #7254, #5023, #7509, .T. ) ;
#4455 = VECTOR ( 'NONE', #7008, 1000.000000000000114 ) ;
#4456 = CARTESIAN_POINT ( 'NONE',  ( -35.49969986081099904, -19.50737899243800300, 55.93350807262480373 ) ) ;
#4457 = AXIS2_PLACEMENT_3D ( 'NONE', #12985, #6071, #10523 ) ;
#4458 = CIRCLE ( 'NONE', #1046, 2.500000000000002220 ) ;
#4459 = ORIENTED_EDGE ( 'NONE', *, *, #9627, .F. ) ;
#4460 = AXIS2_PLACEMENT_3D ( 'NONE', #2045, #4491, #1970 ) ;
#4461 = PRODUCT ( 'Insert Torx Screw', 'Insert Torx Screw', '', ( #8569 ) ) ;
#4462 = DIRECTION ( 'NONE',  ( -3.202566417187950042E-16, 0.000000000000000000, 1.000000000000000000 ) ) ;
#4463 = ORIENTED_EDGE ( 'NONE', *, *, #12717, .T. ) ;
#4464 = CARTESIAN_POINT ( 'NONE',  ( 18.53245405280428315, -26.77692695969465220, 39.96206422150100224 ) ) ;
#4465 = ORIENTED_EDGE ( 'NONE', *, *, #14166, .T. ) ;
#4466 = CARTESIAN_POINT ( 'NONE',  ( -15.49969986081092088, -13.50737899243822504, 57.00231026484397745 ) ) ;
#4467 = EDGE_LOOP ( 'NONE', ( #12021, #8122, #3087, #5769 ) ) ;
#4468 = ORIENTED_EDGE ( 'NONE', *, *, #482, .F. ) ;
#4469 = LINE ( 'NONE', #9124, #539 ) ;
#4470 = ORIENTED_EDGE ( 'NONE', *, *, #15043, .T. ) ;
#4471 = CARTESIAN_POINT ( 'NONE',  ( -15.61203582817000068, -106.4047424672253186, -6.741402868119606318 ) ) ;
#4472 = ADVANCED_FACE ( 'NONE', ( #5372 ), #710, .F. ) ;
#4473 = VECTOR ( 'NONE', #13705, 1000.000000000000114 ) ;
#4474 = ADVANCED_FACE ( 'NONE', ( #1558 ), #6210, .F. ) ;
#4475 = DIRECTION ( 'NONE',  ( 0.5975035461963188466, 0.8018662683283437342, 0.000000000000000000 ) ) ;
#4476 = LINE ( 'NONE', #4548, #12709 ) ;
#4477 = CARTESIAN_POINT ( 'NONE',  ( -7.510659772263728051, -44.94657923994442683, 21.45543621087858810 ) ) ;
#4479 = DIRECTION ( 'NONE',  ( 0.000000000000000000, 1.000000000000000000, 1.224646799147350002E-16 ) ) ;
#4478 = CARTESIAN_POINT ( 'NONE',  ( -15.53979317422733786, -13.47750381512840967, 56.85231026484398598 ) ) ;
#4480 = ORIENTED_EDGE ( 'NONE', *, *, #601, .F. ) ;
#4481 = CARTESIAN_POINT ( 'NONE',  ( -9.425865349984700714, -18.82901260770113794, 57.00231026484399166 ) ) ;
#4482 = DIRECTION ( 'NONE',  ( 0.000000000000000000, 2.168404344971008868E-16, -1.000000000000000000 ) ) ;
#4483 = ORIENTED_EDGE ( 'NONE', *, *, #4384, .T. ) ;
#4484 = DIRECTION ( 'NONE',  ( 0.000000000000000000, -1.000000000000000000, -1.224646799147350002E-16 ) ) ;
#4485 = AXIS2_PLACEMENT_3D ( 'NONE', #1751, #10007, #5346 ) ;
#4486 = CIRCLE ( 'NONE', #9115, 9.974999999999999645 ) ;
#4487 = CARTESIAN_POINT ( 'NONE',  ( -16.02889839021359819, -36.52059104800384404, -17.99486483221301114 ) ) ;
#4488 = VECTOR ( 'NONE', #3560, 1000.000000000000114 ) ;
#4489 = DIRECTION ( 'NONE',  ( 8.018662683283438208E-16, -5.975035461963189015E-16, -1.000000000000000000 ) ) ;
#4490 = VERTEX_POINT ( 'NONE', #5224 ) ;
#4491 = DIRECTION ( 'NONE',  ( 0.000000000000000000, -1.000000000000000000, -1.224646799147350002E-16 ) ) ;
#4492 = EDGE_CURVE ( 'NONE', #4102, #34, #9888, .T. ) ;
#4493 = ADVANCED_FACE ( 'NONE', ( #7955 ), #5667, .T. ) ;
#4494 = ADVANCED_FACE ( 'NONE', ( #3074 ), #5357, .T. ) ;
#4495 = CARTESIAN_POINT ( 'NONE',  ( 7.500300139189000070, -37.00737899243799944, -10.11609617439569675 ) ) ;
#4496 = CARTESIAN_POINT ( 'NONE',  ( -6.468284635389320414, -17.74225372801456757, 57.00231026484399166 ) ) ;
#4497 = EDGE_CURVE ( 'NONE', #13689, #15033, #15080, .T. ) ;
#4498 = CARTESIAN_POINT ( 'NONE',  ( -5.898712304418586960, -10.80152183767200391, 54.00231026484399166 ) ) ;
#4499 = CARTESIAN_POINT ( 'NONE',  ( -17.73437360760467030, -13.24520873212868644, 51.25231026484399166 ) ) ;
#4500 = VERTEX_POINT ( 'NONE', #13790 ) ;
#4501 = CYLINDRICAL_SURFACE ( 'NONE', #13623, 2.500000000000000444 ) ;
#4502 = CARTESIAN_POINT ( 'NONE',  ( -35.48358900502676505, 6.179576214079514962, 29.75589804712084074 ) ) ;
#4503 = VECTOR ( 'NONE', #12133, 1000.000000000000000 ) ;
#4504 = FACE_OUTER_BOUND ( 'NONE', #9754, .T. ) ;
#4505 = CARTESIAN_POINT ( 'NONE',  ( -15.49969986081099904, -32.00737899243800655, 61.71206422150100224 ) ) ;
#4506 = ORIENTED_EDGE ( 'NONE', *, *, #12044, .F. ) ;
#4507 = LINE ( 'NONE', #7780, #6189 ) ;
#4508 = ORIENTED_EDGE ( 'NONE', *, *, #8527, .F. ) ;
#4509 = VECTOR ( 'NONE', #14199, 1000.000000000000114 ) ;
#4510 = DIRECTION ( 'NONE',  ( 0.5975035461963188466, 0.8018662683283437342, 0.000000000000000000 ) ) ;
#4511 = DIRECTION ( 'NONE',  ( 0.8018662683283437342, -0.5975035461963188466, 9.999999999999996833E-16 ) ) ;
#4512 = ADVANCED_FACE ( 'NONE', ( #12490 ), #4532, .F. ) ;
#4513 = EDGE_CURVE ( 'NONE', #3128, #14077, #7728, .T. ) ;
#4514 = ADVANCED_FACE ( 'NONE', ( #6577 ), #5592, .F. ) ;
#4515 = LINE ( 'NONE', #13843, #4455 ) ;
#4516 = CARTESIAN_POINT ( 'NONE',  ( -8.835531075157819103, -48.93602667744891477, 45.18199390436557650 ) ) ;
#4517 =( BOUNDED_CURVE ( )  B_SPLINE_CURVE ( 3, ( #4110, #13308, #8546, #4038 ),
 .UNSPECIFIED., .F., .F. ) 
 B_SPLINE_CURVE_WITH_KNOTS ( ( 4, 4 ),
 ( 3.141592653589793560, 4.400121501412660230 ),
 .UNSPECIFIED. ) 
 CURVE ( )  GEOMETRIC_REPRESENTATION_ITEM ( )  RATIONAL_B_SPLINE_CURVE ( ( 1.000000000000000000, 0.8723071003127499390, 0.8723071003127499390, 1.000000000000000000 ) ) 
 REPRESENTATION_ITEM ( '' )  );
#4518 = LINE ( 'NONE', #6564, #12379 ) ;
#4519 = AXIS2_PLACEMENT_3D ( 'NONE', #11134, #507, #4247 ) ;
#4520 = CARTESIAN_POINT ( 'NONE',  ( -28.78282149594069850, -32.00737899243799944, -10.85656391856669778 ) ) ;
#4521 = PLANE ( 'NONE',  #940 ) ;
#4522 = EDGE_CURVE ( 'NONE', #11878, #9733, #1649, .T. ) ;
#4523 = DIRECTION ( 'NONE',  ( 0.000000000000000000, 0.000000000000000000, -1.000000000000000000 ) ) ;
#4524 = EDGE_LOOP ( 'NONE', ( #2115, #5739, #1062, #14717 ) ) ;
#4525 = CARTESIAN_POINT ( 'NONE',  ( -9.499699860810959962, -67.00737899243799234, -5.497689735155994128 ) ) ;
#4526 = ORIENTED_EDGE ( 'NONE', *, *, #12420, .F. ) ;
#4528 = ORIENTED_EDGE ( 'NONE', *, *, #14088, .T. ) ;
#4527 = CARTESIAN_POINT ( 'NONE',  ( 13.85920135429429934, -23.75737899243800300, 24.21206422150099868 ) ) ;
#4529 = ORIENTED_EDGE ( 'NONE', *, *, #1798, .T. ) ;
#4530 = CARTESIAN_POINT ( 'NONE',  ( -13.18491133144367922, -15.23222315862922471, 56.75231026484399166 ) ) ;
#4531 = VERTEX_POINT ( 'NONE', #784 ) ;
#4532 = PLANE ( 'NONE',  #6810 ) ;
#4533 = CIRCLE ( 'NONE', #8665, 19.00000000000000000 ) ;
#4534 = LINE ( 'NONE', #6882, #7338 ) ;
#4535 = VERTEX_POINT ( 'NONE', #4608 ) ;
#4536 = EDGE_CURVE ( 'NONE', #7739, #13230, #4635, .T. ) ;
#4537 = CARTESIAN_POINT ( 'NONE',  ( -19.04823043207872502, -51.68209199896817552, -17.83013874036776514 ) ) ;
#4538 = ORIENTED_EDGE ( 'NONE', *, *, #334, .F. ) ;
#4539 = CARTESIAN_POINT ( 'NONE',  ( 16.32012704356523614, -23.84468502132440904, 44.06002385016308409 ) ) ;
#4540 = ORIENTED_EDGE ( 'NONE', *, *, #3060, .T. ) ;
#4541 = VECTOR ( 'NONE', #5118, 1000.000000000000000 ) ;
#4542 = DIRECTION ( 'NONE',  ( -3.632077277826439854E-16, 1.000000000000000000, 0.000000000000000000 ) ) ;
#4543 = ORIENTED_EDGE ( 'NONE', *, *, #13379, .F. ) ;
#4544 = ORIENTED_EDGE ( 'NONE', *, *, #13083, .F. ) ;
#4545 = CYLINDRICAL_SURFACE ( 'NONE', #13253, 37.50000000000000000 ) ;
#4546 = VERTEX_POINT ( 'NONE', #1010 ) ;
#4547 = DIRECTION ( 'NONE',  ( -0.5975035461963187355, -0.8018662683283438453, 0.000000000000000000 ) ) ;
#4548 = CARTESIAN_POINT ( 'NONE',  ( -11.61446667642527331, -19.42012692406430574, 56.85231026484400019 ) ) ;
#4549 = CIRCLE ( 'NONE', #3073, 9.974999999999999645 ) ;
#4550 = FACE_OUTER_BOUND ( 'NONE', #12730, .T. ) ;
#4551 = EDGE_CURVE ( 'NONE', #1400, #6240, #9033, .T. ) ;
#4553 = CARTESIAN_POINT ( 'NONE',  ( -34.99969986081099904, -20.37340439622244048, -12.21913358627979918 ) ) ;
#4552 = CARTESIAN_POINT ( 'NONE',  ( -14.11952815701478059, -21.46390939632912875, 56.85231026484400019 ) ) ;
#4554 = ORIENTED_EDGE ( 'NONE', *, *, #6254, .T. ) ;
#4555 = CYLINDRICAL_SURFACE ( 'NONE', #201, 19.00000000000000000 ) ;
#4556 = PLANE ( 'NONE',  #12550 ) ;
#4557 = ORIENTED_EDGE ( 'NONE', *, *, #13124, .T. ) ;
#4558 = ORIENTED_EDGE ( 'NONE', *, *, #9314, .F. ) ;
#4559 = DIRECTION ( 'NONE',  ( -1.000000000000000000, -1.201369187114119994E-15, -9.616040805000176517E-16 ) ) ;
#4560 = EDGE_CURVE ( 'NONE', #5342, #6219, #10262, .T. ) ;
#4561 = CARTESIAN_POINT ( 'NONE',  ( -23.49969986081100259, -44.50737899243799944, -17.13441993860073254 ) ) ;
#4562 = AXIS2_PLACEMENT_3D ( 'NONE', #14151, #2518, #13923 ) ;
#4563 = CARTESIAN_POINT ( 'NONE',  ( -24.03943920472178775, -16.57887731378902885, 57.00231026484397745 ) ) ;
#4564 = ORIENTED_EDGE ( 'NONE', *, *, #5519, .T. ) ;
#4565 = DIRECTION ( 'NONE',  ( 8.018662683283438208E-16, -5.975035461963189015E-16, -1.000000000000000000 ) ) ;
#4566 = VECTOR ( 'NONE', #15015, 1000.000000000000000 ) ;
#4567 = CARTESIAN_POINT ( 'NONE',  ( -6.426265323245524463, -13.69186664111786023, 57.00231026484399166 ) ) ;
#4568 = CONTEXT_DEPENDENT_SHAPE_REPRESENTATION ( #12319, #3964 ) ;
#4569 = VECTOR ( 'NONE', #306, 1000.000000000000000 ) ;
#4570 = CARTESIAN_POINT ( 'NONE',  ( -29.57393575939414632, -54.93314309385485217, -15.32525311590548966 ) ) ;
#4571 = EDGE_CURVE ( 'NONE', #11290, #2975, #8037, .T. ) ;
#4572 = DIRECTION ( 'NONE',  ( 0.7953815700667045130, 0.6061090314441981430, 2.756373558170028881E-16 ) ) ;
#4573 = ORIENTED_EDGE ( 'NONE', *, *, #11880, .F. ) ;
#4574 = CARTESIAN_POINT ( 'NONE',  ( -10.31310630199996403, -90.56276996998271045, -4.100613025930020861 ) ) ;
#4575 = EDGE_CURVE ( 'NONE', #1508, #6681, #12700, .T. ) ;
#4576 = DIRECTION ( 'NONE',  ( 1.000000000000000000, -1.291538348938060198E-32, 1.054621095516909827E-16 ) ) ;
#4577 = VECTOR ( 'NONE', #517, 1000.000000000000000 ) ;
#4578 = EDGE_CURVE ( 'NONE', #9643, #5814, #11338, .T. ) ;
#4579 = FACE_OUTER_BOUND ( 'NONE', #10615, .T. ) ;
#4580 = EDGE_LOOP ( 'NONE', ( #95, #7669, #2167, #6083 ) ) ;
#4581 = FACE_OUTER_BOUND ( 'NONE', #10267, .T. ) ;
#4582 = ORIENTED_EDGE ( 'NONE', *, *, #5868, .T. ) ;
#4583 = DIRECTION ( 'NONE',  ( -0.01206535623792160013, -0.9999272109403024578, 5.877852522924710079E-16 ) ) ;
#4584 = LINE ( 'NONE', #152, #12416 ) ;
#4585 = VECTOR ( 'NONE', #6623, 1000.000000000000000 ) ;
#4586 = EDGE_CURVE ( 'NONE', #1150, #12465, #14929, .T. ) ;
#4587 = CIRCLE ( 'NONE', #10699, 0.4500000000000011768 ) ;
#4588 = FACE_OUTER_BOUND ( 'NONE', #9985, .T. ) ;
#4589 = CARTESIAN_POINT ( 'NONE',  ( 9.000300139189000959, -27.00737899243800300, 5.212064221501000461 ) ) ;
#4590 = LINE ( 'NONE', #14225, #12138 ) ;
#4591 = DIRECTION ( 'NONE',  ( -0.3956847857120157075, 0.9183863840214729901, -8.660254037844388394E-16 ) ) ;
#4592 = EDGE_CURVE ( 'NONE', #10639, #1735, #14648, .T. ) ;
#4593 = ADVANCED_FACE ( 'NONE', ( #5517 ), #10179, .T. ) ;
#4594 = AXIS2_PLACEMENT_3D ( 'NONE', #6182, #14307, #7329 ) ;
#4595 = AXIS2_PLACEMENT_3D ( 'NONE', #7520, #10973, #9751 ) ;
#4596 = CARTESIAN_POINT ( 'NONE',  ( -33.37651573321840459, -23.18484177525213497, 57.27215087687875439 ) ) ;
#4597 = DIRECTION ( 'NONE',  ( -8.018662683283438208E-16, 5.975035461963189015E-16, 1.000000000000000000 ) ) ;
#4598 = AXIS2_PLACEMENT_3D ( 'NONE', #10727, #12028, #252 ) ;
#4599 = ORIENTED_EDGE ( 'NONE', *, *, #10543, .T. ) ;
#4600 = DIRECTION ( 'NONE',  ( -8.660254037844387408E-16, 0.8660254037844387076, 0.4999999999999998890 ) ) ;
#4601 = ORIENTED_EDGE ( 'NONE', *, *, #740, .F. ) ;
#4603 = ORIENTED_EDGE ( 'NONE', *, *, #4755, .T. ) ;
#4602 = CARTESIAN_POINT ( 'NONE',  ( -25.33132850951382053, -11.70608228131975892, 60.40032490398561293 ) ) ;
#4604 = EDGE_LOOP ( 'NONE', ( #12968, #5174, #9689, #14944 ) ) ;
#4605 = CARTESIAN_POINT ( 'NONE',  ( -15.49969986081099904, 22.99262100756200056, 24.21206422150100224 ) ) ;
#4606 = VERTEX_POINT ( 'NONE', #11712 ) ;
#4607 =( BOUNDED_CURVE ( )  B_SPLINE_CURVE ( 3, ( #13210, #2714, #7367, #12053 ),
 .UNSPECIFIED., .F., .F. ) 
 B_SPLINE_CURVE_WITH_KNOTS ( ( 4, 4 ),
 ( 1.570796326794895004, 3.141592653589793560 ),
 .UNSPECIFIED. ) 
 CURVE ( )  GEOMETRIC_REPRESENTATION_ITEM ( )  RATIONAL_B_SPLINE_CURVE ( ( 1.000000000000000000, 0.8047378541243644934, 0.8047378541243644934, 1.000000000000000000 ) ) 
 REPRESENTATION_ITEM ( '' )  );
#4608 = CARTESIAN_POINT ( 'NONE',  ( 4.000300139189000959, -19.50737899243798879, 51.53354502093799994 ) ) ;
#4609 = CARTESIAN_POINT ( 'NONE',  ( -20.87112600995945755, -108.0608273576312968, -5.497689735156002122 ) ) ;
#4610 = FACE_OUTER_BOUND ( 'NONE', #2522, .T. ) ;
#4611 = SHAPE_REPRESENTATION_RELATIONSHIP ( 'NONE' , 'NONE' ,  #6151, #4622 ) ;
#4612 = DIRECTION ( 'NONE',  ( -1.000000000000000000, 3.922012711866029438E-32, -3.202566417187950042E-16 ) ) ;
#4613 = ORIENTED_EDGE ( 'NONE', *, *, #11882, .T. ) ;
#4614 = EDGE_CURVE ( 'NONE', #13499, #11960, #11947, .T. ) ;
#4615 = CARTESIAN_POINT ( 'NONE',  ( 6.912059853347208183, -37.03279448458209089, -10.56576583290206806 ) ) ;
#4616 = ORIENTED_EDGE ( 'NONE', *, *, #1521, .T. ) ;
#4617 = ORIENTED_EDGE ( 'NONE', *, *, #5399, .T. ) ;
#4618 = VERTEX_POINT ( 'NONE', #14169 ) ;
#4619 = CARTESIAN_POINT ( 'NONE',  ( -15.49969986081100082, 10.73810275766729561, 24.21206422150099868 ) ) ;
#4620 = ORIENTED_EDGE ( 'NONE', *, *, #1987, .F. ) ;
#4621 = CARTESIAN_POINT ( 'NONE',  ( -20.31756358285883479, -22.27118552192390055, 56.69196217374378222 ) ) ;
#4622 = ADVANCED_BREP_SHAPE_REPRESENTATION ( '', ( #2515, #6789 ), #8750 ) ;
#4623 = VECTOR ( 'NONE', #13558, 1000.000000000000000 ) ;
#4624 = EDGE_CURVE ( 'NONE', #2831, #12009, #14013, .T. ) ;
#4625 = AXIS2_PLACEMENT_3D ( 'NONE', #11950, #1468, #7032 ) ;
#4626 = EDGE_CURVE ( 'NONE', #1378, #6204, #12956, .T. ) ;
#4627 = PLANE ( 'NONE',  #11601 ) ;
#4628 = CARTESIAN_POINT ( 'NONE',  ( -15.49969986081099904, 0.9926210075619958939, 47.21206422150099513 ) ) ;
#4629 = VECTOR ( 'NONE', #8788, 1000.000000000000000 ) ;
#4630 = CARTESIAN_POINT ( 'NONE',  ( -7.512043759983883184, -44.96869557946827456, 21.47290527092978607 ) ) ;
#4632 = DIRECTION ( 'NONE',  ( 0.000000000000000000, 0.000000000000000000, 1.000000000000000000 ) ) ;
#4631 = CARTESIAN_POINT ( 'NONE',  ( -15.49969986081099904, -13.50737899243800122, 61.71206422150099513 ) ) ;
#4633 = VERTEX_POINT ( 'NONE', #1313 ) ;
#4634 = CARTESIAN_POINT ( 'NONE',  ( -7.705200311943016800, -46.31941204765107045, 42.00231026484399166 ) ) ;
#4635 = CIRCLE ( 'NONE', #2187, 0.2000000000000012046 ) ;
#4636 = CARTESIAN_POINT ( 'NONE',  ( -19.07799122369186762, -16.25188662377412641, -13.11718427892139438 ) ) ;
#4637 = ORIENTED_EDGE ( 'NONE', *, *, #1880, .F. ) ;
#4638 = AXIS2_PLACEMENT_3D ( 'NONE', #9072, #4724, #11376 ) ;
#4639 = ORIENTED_EDGE ( 'NONE', *, *, #8932, .F. ) ;
#4640 = CARTESIAN_POINT ( 'NONE',  ( -15.61203582817000068, -106.9748017008338365, -5.104852750214476487 ) ) ;
#4641 = CARTESIAN_POINT ( 'NONE',  ( -18.36422177163696290, -5.957162821864243618, 57.00231026484397745 ) ) ;
#4642 = ORIENTED_EDGE ( 'NONE', *, *, #1720, .F. ) ;
#4643 = ORIENTED_EDGE ( 'NONE', *, *, #12823, .T. ) ;
#4644 = DIRECTION ( 'NONE',  ( -8.018662683283438208E-16, 5.975035461963189015E-16, 1.000000000000000000 ) ) ;
#4645 = ADVANCED_FACE ( 'NONE', ( #3530 ), #2537, .F. ) ;
#4646 = DIRECTION ( 'NONE',  ( -1.000000000000000000, 0.000000000000000000, 0.000000000000000000 ) ) ;
#4647 = ITEM_DEFINED_TRANSFORMATION ( 'NONE', 'NONE', #7303,  #6789 ) ;
#4648 = LINE ( 'NONE', #9302, #5797 ) ;
#4649 = DIRECTION ( 'NONE',  ( 1.000000000000000000, -1.499759782661860071E-32, 1.224646799147350002E-16 ) ) ;
#4650 = LINE ( 'NONE', #6772, #368 ) ;
#4652 = ORIENTED_EDGE ( 'NONE', *, *, #14304, .F. ) ;
#4651 = VECTOR ( 'NONE', #1785, 1000.000000000000114 ) ;
#4653 = CARTESIAN_POINT ( 'NONE',  ( -10.32812483352770450, -90.56483419681595137, -4.046006962230706883 ) ) ;
#4654 = PLANE ( 'NONE',  #9453 ) ;
#4655 = CARTESIAN_POINT ( 'NONE',  ( -22.00391959472895209, -7.178368354675633611, 57.00231026484397745 ) ) ;
#4656 = ORIENTED_EDGE ( 'NONE', *, *, #14021, .T. ) ;
#4657 = PLANE ( 'NONE',  #2781 ) ;
#4658 = ORIENTED_EDGE ( 'NONE', *, *, #13424, .T. ) ;
#4659 = LINE ( 'NONE', #6015, #11534 ) ;
#4660 = DIRECTION ( 'NONE',  ( -8.018662683283438208E-16, 5.975035461963189015E-16, 1.000000000000000000 ) ) ;
#4661 = ADVANCED_FACE ( 'NONE', ( #8341 ), #21, .T. ) ;
#4662 = VECTOR ( 'NONE', #13941, 1000.000000000000000 ) ;
#4663 = LINE ( 'NONE', #7085, #2748 ) ;
#4664 = CARTESIAN_POINT ( 'NONE',  ( -15.49969986081099904, 22.99262100756199700, 40.08706422150100224 ) ) ;
#4665 = ADVANCED_FACE ( 'NONE', ( #1387 ), #2313, .F. ) ;
#4666 = CARTESIAN_POINT ( 'NONE',  ( -17.81448839017816610, -11.78253482624722004, 51.10586365543726117 ) ) ;
#4667 = DIRECTION ( 'NONE',  ( 8.018662683283438208E-16, -5.975035461963189015E-16, -1.000000000000000000 ) ) ;
#4668 = CARTESIAN_POINT ( 'NONE',  ( -7.773685182324116205, -47.89679818372221831, -7.581023005281736005 ) ) ;
#4669 = CARTESIAN_POINT ( 'NONE',  ( -20.86311301939802831, -108.2285642389760483, -5.850193701754826670 ) ) ;
#4670 = CARTESIAN_POINT ( 'NONE',  ( -14.19354049678269192, -21.47604090745013750, 56.85231026484400019 ) ) ;
#4671 = ORIENTED_EDGE ( 'NONE', *, *, #740, .T. ) ;
#4672 = CARTESIAN_POINT ( 'NONE',  ( -5.499699860810998153, -46.50737899243799944, -2.497689735156003010 ) ) ;
#4673 = PRODUCT_DEFINITION_CONTEXT ( 'detailed design', #2935, 'design' ) ;
#4674 = EDGE_LOOP ( 'NONE', ( #12620, #4278 ) ) ;
#4675 = EDGE_CURVE ( 'NONE', #7160, #2925, #7049, .T. ) ;
#4677 = VERTEX_POINT ( 'NONE', #6037 ) ;
#4676 = DIRECTION ( 'NONE',  ( 0.5975035461963189576, 0.8018662683283437342, 0.000000000000000000 ) ) ;
#4678 = ORIENTED_EDGE ( 'NONE', *, *, #918, .F. ) ;
#4679 = CARTESIAN_POINT ( 'NONE',  ( -15.54961651457173488, -13.51026476396819831, 56.85231026484398598 ) ) ;
#4680 = EDGE_LOOP ( 'NONE', ( #7542, #13737, #2036, #10008 ) ) ;
#4681 = CARTESIAN_POINT ( 'NONE',  ( -15.49969986081092088, -13.50737899243822504, 57.00231026484397745 ) ) ;
#4682 = EDGE_CURVE ( 'NONE', #4722, #14217, #9568, .T. ) ;
#4683 = EDGE_CURVE ( 'NONE', #4771, #7197, #9417, .T. ) ;
#4684 = CARTESIAN_POINT ( 'NONE',  ( -20.00744539586189319, -5.630737564061013778, 56.85231026484398598 ) ) ;
#4685 = CIRCLE ( 'NONE', #13244, 0.2000000000000012046 ) ;
#4686 = EDGE_CURVE ( 'NONE', #3306, #5040, #6950, .T. ) ;
#4687 = LINE ( 'NONE', #3609, #14186 ) ;
#4688 = DIRECTION ( 'NONE',  ( 1.000000000000000000, 0.000000000000000000, 0.000000000000000000 ) ) ;
#4689 = LINE ( 'NONE', #479, #10457 ) ;
#4690 = LINE ( 'NONE', #3537, #9878 ) ;
#4691 = CARTESIAN_POINT ( 'NONE',  ( -16.02307658328272311, -52.50737899243798523, -17.99768973515599413 ) ) ;
#4692 = CIRCLE ( 'NONE', #7361, 0.1500000000000015488 ) ;
#4693 = ORIENTED_EDGE ( 'NONE', *, *, #15084, .F. ) ;
#4694 = CARTESIAN_POINT ( 'NONE',  ( 3.284438305224395283, -39.31204358972114932, -12.95406313883616356 ) ) ;
#4695 = ORIENTED_EDGE ( 'NONE', *, *, #9145, .F. ) ;
#4696 = CARTESIAN_POINT ( 'NONE',  ( -11.67714598312096008, -19.46131314156662384, 57.00231026484399166 ) ) ;
#4697 = ORIENTED_EDGE ( 'NONE', *, *, #6057, .T. ) ;
#4698 = ORIENTED_EDGE ( 'NONE', *, *, #11102, .F. ) ;
#4699 = CARTESIAN_POINT ( 'NONE',  ( 4.095996200104924156, -38.34531428877323123, 51.47509614191934446 ) ) ;
#4700 = ORIENTED_EDGE ( 'NONE', *, *, #12809, .F. ) ;
#4701 = CARTESIAN_POINT ( 'NONE',  ( -15.64858178355719964, -107.1622034095870077, -6.087689735155999315 ) ) ;
#4702 = EDGE_CURVE ( 'NONE', #4749, #12994, #3762, .T. ) ;
#4703 = CARTESIAN_POINT ( 'NONE',  ( -11.02342383152547356, -36.50737899243797102, -13.49768973515603321 ) ) ;
#4704 = VECTOR ( 'NONE', #9987, 1000.000000000000000 ) ;
#4705 = DIRECTION ( 'NONE',  ( 8.018662683283438208E-16, -5.975035461963189015E-16, -1.000000000000000000 ) ) ;
#4706 = AXIS2_PLACEMENT_3D ( 'NONE', #11944, #6338, #13098 ) ;
#4707 = VECTOR ( 'NONE', #9699, 1000.000000000000000 ) ;
#4708 = VECTOR ( 'NONE', #8939, 1000.000000000000000 ) ;
#4709 = CARTESIAN_POINT ( 'NONE',  ( -7.504323356601999784, -44.76276341930999081, 21.29631823119984091 ) ) ;
#4711 = CARTESIAN_POINT ( 'NONE',  ( -17.81448839017816610, -11.78253482624722537, 51.25231026484399166 ) ) ;
#4710 = DIRECTION ( 'NONE',  ( -8.018662683283438208E-16, 5.975035461963189015E-16, 1.000000000000000000 ) ) ;
#4712 = ORIENTED_EDGE ( 'NONE', *, *, #2386, .F. ) ;
#4713 = CYLINDRICAL_SURFACE ( 'NONE', #6041, 8.000000000000000000 ) ;
#4714 = DIRECTION ( 'NONE',  ( 0.000000000000000000, 1.224646799147350002E-16, -1.000000000000000000 ) ) ;
#4715 = VERTEX_POINT ( 'NONE', #5968 ) ;
#4716 = ORIENTED_EDGE ( 'NONE', *, *, #6896, .T. ) ;
#4717 = EDGE_CURVE ( 'NONE', #15034, #7782, #4132, .T. ) ;
#4718 = CARTESIAN_POINT ( 'NONE',  ( -5.499699860810998153, -46.50737899243799944, -5.497689735156003010 ) ) ;
#4719 = ORIENTED_EDGE ( 'NONE', *, *, #3707, .T. ) ;
#4720 = AXIS2_PLACEMENT_3D ( 'NONE', #10817, #6055, #348 ) ;
#4721 = CARTESIAN_POINT ( 'NONE',  ( -14.97186396627019533, -36.50737899243800655, -17.99768973515599768 ) ) ;
#4722 = VERTEX_POINT ( 'NONE', #1234 ) ;
#4723 = AXIS2_PLACEMENT_3D ( 'NONE', #12176, #8573, #11101 ) ;
#4724 = DIRECTION ( 'NONE',  ( -0.4274949678123940999, 0.9040177279761056894, -8.829475928589322242E-16 ) ) ;
#4725 = AXIS2_PLACEMENT_3D ( 'NONE', #6186, #14312, #12867 ) ;
#4726 = CARTESIAN_POINT ( 'NONE',  ( -11.61446667642527331, -19.42012692406430574, 56.85231026484400019 ) ) ;
#4727 = CARTESIAN_POINT ( 'NONE',  ( -20.18599136182623965, -36.50737899243796392, -13.49768973515603498 ) ) ;
#4728 = ORIENTED_EDGE ( 'NONE', *, *, #5985, .F. ) ;
#4729 = AXIS2_PLACEMENT_3D ( 'NONE', #9841, #4253, #7534 ) ;
#4730 = CARTESIAN_POINT ( 'NONE',  ( -3.508527451665000463, -45.20834088676133433, -4.747689735156000346 ) ) ;
#4731 = ORIENTED_EDGE ( 'NONE', *, *, #10381, .T. ) ;
#4732 = EDGE_CURVE ( 'NONE', #337, #12833, #14086, .T. ) ;
#4733 = DIRECTION ( 'NONE',  ( 0.5104125104779002609, 0.8599296884906623140, -1.045284632676510365E-16 ) ) ;
#4734 = ORIENTED_EDGE ( 'NONE', *, *, #12370, .T. ) ;
#4735 = DIRECTION ( 'NONE',  ( 0.5975035461963188466, 0.8018662683283437342, 0.000000000000000000 ) ) ;
#4736 = ORIENTED_EDGE ( 'NONE', *, *, #4279, .F. ) ;
#4737 = DIRECTION ( 'NONE',  ( 0.000000000000000000, 0.1872998510044521503, 0.9823027872370667657 ) ) ;
#4738 = CARTESIAN_POINT ( 'NONE',  ( -15.49969986081092088, -13.50737899243822504, 57.00231026484397745 ) ) ;
#4739 = VECTOR ( 'NONE', #9918, 1000.000000000000114 ) ;
#4740 = PLANE ( 'NONE',  #11538 ) ;
#4741 = LINE ( 'NONE', #11546, #5483 ) ;
#4742 = CARTESIAN_POINT ( 'NONE',  ( -5.840324169876037530, -16.14984675272692627, 60.44710126137897532 ) ) ;
#4743 = VECTOR ( 'NONE', #2937, 1000.000000000000000 ) ;
#4744 = DIRECTION ( 'NONE',  ( 0.9320450512859425052, 0.3618458327180909539, -0.01896353653557691574 ) ) ;
#4745 = CARTESIAN_POINT ( 'NONE',  ( -10.85342163307452523, -20.71489927548028476, 56.85231026484400019 ) ) ;
#4746 = DIRECTION ( 'NONE',  ( 0.09252159378507134047, -0.9957106782009873536, 6.691306063588577540E-16 ) ) ;
#4747 = AXIS2_PLACEMENT_3D ( 'NONE', #7034, #5976, #8268 ) ;
#4748 = ADVANCED_FACE ( 'NONE', ( #7349 ), #2620, .T. ) ;
#4749 = VERTEX_POINT ( 'NONE', #11959 ) ;
#4750 = CARTESIAN_POINT ( 'NONE',  ( 7.200737182676100190, 4.873818854045000037, 20.51204286552489009 ) ) ;
#4751 = VERTEX_POINT ( 'NONE', #1550 ) ;
#4753 = ORIENTED_EDGE ( 'NONE', *, *, #13475, .T. ) ;
#4752 = DIRECTION ( 'NONE',  ( 1.000000000000000000, -1.291538348938060198E-32, 1.054621095516909827E-16 ) ) ;
#4754 = EDGE_LOOP ( 'NONE', ( #6982, #14620, #11516, #3996, #5037, #299, #8579, #2191, #11800, #6654, #5308, #11086 ) ) ;
#4755 = EDGE_CURVE ( 'NONE', #14491, #5023, #1477, .T. ) ;
#4756 = CARTESIAN_POINT ( 'NONE',  ( -25.45346213993001783, -14.15794911993139849, 57.00231026484397745 ) ) ;
#4757 = ORIENTED_EDGE ( 'NONE', *, *, #198, .F. ) ;
#4758 = AXIS2_PLACEMENT_3D ( 'NONE', #3855, #2481, #7363 ) ;
#4759 = DIRECTION ( 'NONE',  ( 8.018662683283438208E-16, -5.975035461963189015E-16, -1.000000000000000000 ) ) ;
#4760 = LINE ( 'NONE', #4838, #2085 ) ;
#4761 = CONICAL_SURFACE ( 'NONE', #11353, 2.000000000000001776, 0.7853981633974476129 ) ;
#4762 = CARTESIAN_POINT ( 'NONE',  ( -15.49969986081099904, 71.39262100756199914, 24.21206422150100579 ) ) ;
#4763 = DIRECTION ( 'NONE',  ( 0.000000000000000000, 0.000000000000000000, 1.000000000000000000 ) ) ;
#4764 = CARTESIAN_POINT ( 'NONE',  ( -17.75327345881522234, -9.601260756853328360, -13.22096152104317568 ) ) ;
#4765 = DIRECTION ( 'NONE',  ( 8.018662683283438208E-16, -5.975035461963189015E-16, -1.000000000000000000 ) ) ;
#4766 = DIRECTION ( 'NONE',  ( -0.9183863840214728791, -0.3956847857120156520, -4.999999999999998416E-16 ) ) ;
#4767 = EDGE_CURVE ( 'NONE', #4359, #15022, #1772, .T. ) ;
#4768 = ORIENTED_EDGE ( 'NONE', *, *, #729, .T. ) ;
#4769 = CARTESIAN_POINT ( 'NONE',  ( 2.819042285013538596, -40.24211141612355647, -13.21890428332254963 ) ) ;
#4770 = EDGE_CURVE ( 'NONE', #5960, #12566, #341, .T. ) ;
#4771 = VERTEX_POINT ( 'NONE', #13410 ) ;
#4772 = ORIENTED_EDGE ( 'NONE', *, *, #14611, .T. ) ;
#4773 = ORIENTED_EDGE ( 'NONE', *, *, #9247, .T. ) ;
#4774 = VECTOR ( 'NONE', #10568, 1000.000000000000114 ) ;
#4775 = EDGE_CURVE ( 'NONE', #5903, #633, #11219, .T. ) ;
#4776 = DIRECTION ( 'NONE',  ( -0.5491495666976170531, 0.8357240892757724637, -9.396926207859082113E-16 ) ) ;
#4777 = ORIENTED_EDGE ( 'NONE', *, *, #9257, .T. ) ;
#4778 = LINE ( 'NONE', #5008, #10820 ) ;
#4779 = EDGE_CURVE ( 'NONE', #5304, #13197, #1697, .T. ) ;
#4780 = FACE_OUTER_BOUND ( 'NONE', #9505, .T. ) ;
#4781 = DIRECTION ( 'NONE',  ( 0.5975035461963189576, 0.8018662683283437342, 0.000000000000000000 ) ) ;
#4783 = EDGE_CURVE ( 'NONE', #14533, #6892, #12181, .T. ) ;
#4782 =( BOUNDED_CURVE ( )  B_SPLINE_CURVE ( 3, ( #2735, #7392, #10536, #69 ),
 .UNSPECIFIED., .F., .F. ) 
 B_SPLINE_CURVE_WITH_KNOTS ( ( 4, 4 ),
 ( 5.266983419591695359, 7.299387194767472664 ),
 .UNSPECIFIED. ) 
 CURVE ( )  GEOMETRIC_REPRESENTATION_ITEM ( )  RATIONAL_B_SPLINE_CURVE ( ( 1.000000000000000000, 0.6843990470536871484, 0.6843990470536871484, 1.000000000000000000 ) ) 
 REPRESENTATION_ITEM ( '' )  );
#4784 = DIRECTION ( 'NONE',  ( -0.5975035461963187355, -0.8018662683283439563, 0.000000000000000000 ) ) ;
#4786 = LINE ( 'NONE', #14041, #8019 ) ;
#4785 = CARTESIAN_POINT ( 'NONE',  ( -7.658052939403637183, -48.44202655475368857, -3.914257181409824593 ) ) ;
#4787 = ORIENTED_EDGE ( 'NONE', *, *, #8377, .T. ) ;
#4788 = PLANE ( 'NONE',  #14842 ) ;
#4789 = EDGE_CURVE ( 'NONE', #1815, #14119, #3213, .T. ) ;
#4790 = DIRECTION ( 'NONE',  ( 0.000000000000000000, 2.168404344971008868E-16, -1.000000000000000000 ) ) ;
#4791 = EDGE_LOOP ( 'NONE', ( #13318, #1713, #4411, #9861 ) ) ;
#4792 = ORIENTED_EDGE ( 'NONE', *, *, #6824, .F. ) ;
#4793 = CARTESIAN_POINT ( 'NONE',  ( 22.00031467284088293, -30.25754668847291384, 24.42409879051542632 ) ) ;
#4794 = CARTESIAN_POINT ( 'NONE',  ( -23.35746721609777055, -42.93911546747612107, 56.16991628440959516 ) ) ;
#4795 = ORIENTED_EDGE ( 'NONE', *, *, #7194, .F. ) ;
#4796 = AXIS2_PLACEMENT_3D ( 'NONE', #2940, #12277, #7810 ) ;
#4797 = VECTOR ( 'NONE', #5711, 1000.000000000000000 ) ;
#4798 = DIRECTION ( 'NONE',  ( 8.018662683283438208E-16, -5.975035461963189015E-16, -1.000000000000000000 ) ) ;
#4799 = PRODUCT_DEFINITION ( 'UNKNOWN', '', #11954, #3444 ) ;
#4800 = EDGE_CURVE ( 'NONE', #12659, #15056, #12685, .T. ) ;
#4801 = DIRECTION ( 'NONE',  ( -8.018662683283438208E-16, 5.975035461963189015E-16, 1.000000000000000000 ) ) ;
#4802 = DIRECTION ( 'NONE',  ( -8.018662683283438208E-16, 5.975035461963189015E-16, 1.000000000000000000 ) ) ;
#4803 = VERTEX_POINT ( 'NONE', #5000 ) ;
#4804 = CYLINDRICAL_SURFACE ( 'NONE', #6274, 0.2000000000000012046 ) ;
#4805 = CARTESIAN_POINT ( 'NONE',  ( -9.884208147447518300, -5.263176313152190922, 57.00231026484397745 ) ) ;
#4806 = VERTEX_POINT ( 'NONE', #9658 ) ;
#4807 = CARTESIAN_POINT ( 'NONE',  ( -15.04562126104788966, -5.444807279564146896, 57.00231026484397745 ) ) ;
#4808 = ORIENTED_EDGE ( 'NONE', *, *, #8077, .T. ) ;
#4809 = CARTESIAN_POINT ( 'NONE',  ( -7.508316264967583642, -44.14096455381468331, -6.326192033447865626 ) ) ;
#4810 = ORIENTED_EDGE ( 'NONE', *, *, #1987, .T. ) ;
#4811 = CARTESIAN_POINT ( 'NONE',  ( -15.50552586659557797, -13.55703840903364288, 56.85231026484398598 ) ) ;
#4812 = CARTESIAN_POINT ( 'NONE',  ( -10.72806301968316411, -20.63252684047564500, 57.00231026484399166 ) ) ;
#4813 = LINE ( 'NONE', #9469, #7524 ) ;
#4814 = CARTESIAN_POINT ( 'NONE',  ( -6.938526287600614850, -8.388108336439911383, 54.00231026484399166 ) ) ;
#4815 = CARTESIAN_POINT ( 'NONE',  ( -36.42585024326830734, 12.65779542994540208, 16.16206422150100153 ) ) ;
#4816 = VECTOR ( 'NONE', #13773, 1000.000000000000000 ) ;
#4817 =( NAMED_UNIT ( * ) SI_UNIT ( $, .STERADIAN. ) SOLID_ANGLE_UNIT ( ) );
#4818 = ADVANCED_FACE ( 'NONE', ( #14330 ), #7301, .F. ) ;
#4819 = EDGE_CURVE ( 'NONE', #569, #2126, #11025, .T. ) ;
#4820 = CARTESIAN_POINT ( 'NONE',  ( -7.985436018829471294, -20.06759727486528178, 57.00231026484399166 ) ) ;
#4821 = VECTOR ( 'NONE', #5307, 1000.000000000000000 ) ;
#4822 = DIRECTION ( 'NONE',  ( 0.000000000000000000, 0.1872998510044759646, 0.9823027872370621028 ) ) ;
#4823 = ORIENTED_EDGE ( 'NONE', *, *, #9988, .T. ) ;
#4824 = CARTESIAN_POINT ( 'NONE',  ( -12.67520354219633383, -51.99671047118290090, -17.89194748959578263 ) ) ;
#4825 = AXIS2_PLACEMENT_3D ( 'NONE', #293, #13304, #444 ) ;
#4826 = CARTESIAN_POINT ( 'NONE',  ( -28.78282149594069850, -31.14135358865360104, 59.28069236156870403 ) ) ;
#4827 = DIRECTION ( 'NONE',  ( 0.8018662683283437342, -0.5975035461963188466, 1.000000000000000078E-15 ) ) ;
#4828 = ORIENTED_EDGE ( 'NONE', *, *, #2804, .T. ) ;
#4829 = DIRECTION ( 'NONE',  ( -8.018662683283438208E-16, 5.975035461963189015E-16, 1.000000000000000000 ) ) ;
#4830 = PRODUCT_DEFINITION_CONTEXT ( 'detailed design', #10258, 'design' ) ;
#4831 = VERTEX_POINT ( 'NONE', #5288 ) ;
#4832 = CIRCLE ( 'NONE', #5080, 37.50000000000000000 ) ;
#4834 = ORIENTED_EDGE ( 'NONE', *, *, #11580, .F. ) ;
#4833 = CARTESIAN_POINT ( 'NONE',  ( -14.61203582816999891, -108.4210244314312916, -5.847664976093791545 ) ) ;
#4835 = ORIENTED_EDGE ( 'NONE', *, *, #7290, .T. ) ;
#4836 = CARTESIAN_POINT ( 'NONE',  ( -15.61203582817000068, -106.1207381828630929, -5.933688532728892184 ) ) ;
#4837 = EDGE_LOOP ( 'NONE', ( #6587, #860, #3926, #7742 ) ) ;
#4838 = CARTESIAN_POINT ( 'NONE',  ( -15.61203582816999891, -107.8822043817477976, -5.237516044744980448 ) ) ;
#4839 = EDGE_CURVE ( 'NONE', #9919, #11420, #1623, .T. ) ;
#4840 = CARTESIAN_POINT ( 'NONE',  ( -9.499699860810929763, -96.50737899243799234, -5.497689735155988799 ) ) ;
#4841 = CIRCLE ( 'NONE', #1652, 0.2000000000000012046 ) ;
#4842 = CARTESIAN_POINT ( 'NONE',  ( 18.30052381647702830, -25.27299409199407521, 7.969642897117474867 ) ) ;
#4843 = AXIS2_PLACEMENT_3D ( 'NONE', #171, #1384, #3684 ) ;
#4844 = FACE_OUTER_BOUND ( 'NONE', #8759, .T. ) ;
#4845 = DIRECTION ( 'NONE',  ( -8.018662683283438208E-16, 5.975035461963189015E-16, 1.000000000000000000 ) ) ;
#4846 = CARTESIAN_POINT ( 'NONE',  ( 3.032897922443514638, -39.75996117776323047, -13.09822540226690357 ) ) ;
#4847 = VERTEX_POINT ( 'NONE', #8577 ) ;
#4848 = CARTESIAN_POINT ( 'NONE',  ( -15.49969986081099371, -57.00737899243799944, -17.99768973515599768 ) ) ;
#4849 = EDGE_LOOP ( 'NONE', ( #5744, #7078, #11085, #12852, #4034, #1311 ) ) ;
#4850 = ORIENTED_EDGE ( 'NONE', *, *, #4003, .F. ) ;
#4851 = DIRECTION ( 'NONE',  ( 1.000000000000000000, 0.000000000000000000, 0.000000000000000000 ) ) ;
#4852 = B_SPLINE_CURVE_WITH_KNOTS ( 'NONE', 3,
 ( #2969, #6475, #1904, #9928, #7628, #13535, #12384, #11158, #677, #12539, #5344, #5562, #13610, #13758, #2056, #9005, #11310, #13685, #8855, #7845, #5492, #11383, #6403 ),
 .UNSPECIFIED., .F., .F.,
 ( 4, 2, 2, 2, 2, 2, 2, 2, 1, 1, 1, 2, 4 ),
 ( 0.1213360741398818166, 0.1630074590234368292, 0.2046788439069918142, 0.2880216136741018396, 0.4547071532083220013, 0.5380499229754320822, 0.5588856154172106017, 0.5614900769724329166, 0.5640945385276554536, 0.5693034616381122959, 0.5797213078590257584, 0.6213926927426793867, 0.7880782322772789117 ),
 .UNSPECIFIED. ) ;
#4853 = PLANE ( 'NONE',  #4207 ) ;
#4854 = EDGE_LOOP ( 'NONE', ( #11500, #14234, #12965, #2157 ) ) ;
#4855 = VECTOR ( 'NONE', #1073, 1000.000000000000000 ) ;
#4856 = PLANE ( 'NONE',  #1540 ) ;
#4857 = EDGE_CURVE ( 'NONE', #7229, #5221, #1071, .T. ) ;
#4858 =( LENGTH_UNIT ( ) NAMED_UNIT ( * ) SI_UNIT ( .MILLI., .METRE. ) );
#4859 = CARTESIAN_POINT ( 'NONE',  ( -10.81589814721888665, -90.65038570870460433, -8.129004277159287639 ) ) ;
#4860 =( GEOMETRIC_REPRESENTATION_CONTEXT ( 3 ) GLOBAL_UNCERTAINTY_ASSIGNED_CONTEXT ( ( #13661 ) ) GLOBAL_UNIT_ASSIGNED_CONTEXT ( ( #14710, #8891, #3310 ) ) REPRESENTATION_CONTEXT ( 'NONE', 'WORKASPACE' ) );
#4861 = ADVANCED_FACE ( 'NONE', ( #10960, #12257 ), #3995, .F. ) ;
#4862 = VECTOR ( 'NONE', #8762, 1000.000000000000227 ) ;
#4863 = DIRECTION ( 'NONE',  ( -0.9183863840214728791, -0.3956847857120156520, -4.999999999999998416E-16 ) ) ;
#4865 = PLANE ( 'NONE',  #13419 ) ;
#4864 = CARTESIAN_POINT ( 'NONE',  ( -7.506424547597141839, -48.98717474752383083, -5.822033054479117453 ) ) ;
#4866 = ORIENTED_EDGE ( 'NONE', *, *, #11826, .T. ) ;
#4867 = LINE ( 'NONE', #9372, #9220 ) ;
#4868 = CYLINDRICAL_SURFACE ( 'NONE', #4057, 0.4500000000000011768 ) ;
#4869 = ORIENTED_EDGE ( 'NONE', *, *, #12574, .F. ) ;
#4870 = EDGE_CURVE ( 'NONE', #7946, #12967, #13836, .T. ) ;
#4871 = ORIENTED_EDGE ( 'NONE', *, *, #6384, .F. ) ;
#4872 = CARTESIAN_POINT ( 'NONE',  ( -15.49969986081099904, -36.50737899243799944, 57.00231026484399877 ) ) ;
#4873 = ORIENTED_EDGE ( 'NONE', *, *, #7572, .F. ) ;
#4874 = AXIS2_PLACEMENT_3D ( 'NONE', #10493, #5886, #4759 ) ;
#4875 = FACE_OUTER_BOUND ( 'NONE', #9143, .T. ) ;
#4876 = ADVANCED_FACE ( 'NONE', ( #14696 ), #1850, .F. ) ;
#4877 = CLOSED_SHELL ( 'NONE', ( #6731, #7399, #4661, #10269, #8764, #13404, #1686, #11748, #5964, #10005, #1973, #2721, #4593, #4173, #7854, #6060, #4861 ) ) ;
#4878 = PLANE ( 'NONE',  #4882 ) ;
#4879 = EDGE_CURVE ( 'NONE', #4535, #9803, #10021, .T. ) ;
#4880 = CARTESIAN_POINT ( 'NONE',  ( -7.145558396657058609, -18.95797028117975103, 57.00231026484399166 ) ) ;
#4881 = AXIS2_PLACEMENT_3D ( 'NONE', #7435, #491, #3002 ) ;
#4882 = AXIS2_PLACEMENT_3D ( 'NONE', #436, #5025, #14280 ) ;
#4883 = DIRECTION ( 'NONE',  ( 0.5975035461963189576, 0.8018662683283437342, 0.000000000000000000 ) ) ;
#4884 = CARTESIAN_POINT ( 'NONE',  ( -15.61203582817000068, -107.5837463816240529, -4.877506371889844594 ) ) ;
#4885 = ORIENTED_EDGE ( 'NONE', *, *, #1824, .F. ) ;
#4886 = CARTESIAN_POINT ( 'NONE',  ( -16.57334897777262483, -22.01522992987520766, 56.85231026484400019 ) ) ;
#4887 = LINE ( 'NONE', #5033, #4082 ) ;
#4888 = ORIENTED_EDGE ( 'NONE', *, *, #9757, .F. ) ;
#4889 = CARTESIAN_POINT ( 'NONE',  ( 9.641860956753800949, -19.50737899243800300, 24.21206422150099868 ) ) ;
#4890 = CARTESIAN_POINT ( 'NONE',  ( -18.04596724311489808, -11.61005040962811563, 57.00231026484397745 ) ) ;
#4891 = ORIENTED_EDGE ( 'NONE', *, *, #4925, .T. ) ;
#4892 = LINE ( 'NONE', #14216, #9377 ) ;
#4893 = VERTEX_POINT ( 'NONE', #2208 ) ;
#4894 = DIRECTION ( 'NONE',  ( -0.1165201156931293391, -0.9931883319083343320, 4.999999999999998416E-16 ) ) ;
#4895 = DIRECTION ( 'NONE',  ( -0.8018662683283437342, 0.5975035461963188466, -1.000000000000000078E-15 ) ) ;
#4896 = VECTOR ( 'NONE', #14652, 1000.000000000000000 ) ;
#4897 = CARTESIAN_POINT ( 'NONE',  ( -14.51048789653087390, -15.80334495249191207, 51.25231026484399166 ) ) ;
#4898 = EDGE_CURVE ( 'NONE', #6978, #6240, #1199, .T. ) ;
#4899 = CARTESIAN_POINT ( 'NONE',  ( -14.61203582816999891, -107.4618831711941169, -7.659374194735305785 ) ) ;
#4900 = CARTESIAN_POINT ( 'NONE',  ( -5.712217893050156370, -15.62993725438619208, 60.41238135938705511 ) ) ;
#4901 = VECTOR ( 'NONE', #3456, 1000.000000000000000 ) ;
#4902 = CARTESIAN_POINT ( 'NONE',  ( 17.66674905504159199, -29.89865791779061865, 6.711258755170492307 ) ) ;
#4903 = LINE ( 'NONE', #2675, #2867 ) ;
#4904 = DIRECTION ( 'NONE',  ( -8.018662683283438208E-16, 5.975035461963189015E-16, 1.000000000000000000 ) ) ;
#4905 = PLANE ( 'NONE',  #565 ) ;
#4906 = VERTEX_POINT ( 'NONE', #2363 ) ;
#4907 = PLANE ( 'NONE',  #14218 ) ;
#4908 = ORIENTED_EDGE ( 'NONE', *, *, #12103, .T. ) ;
#4910 = ORIENTED_EDGE ( 'NONE', *, *, #5064, .F. ) ;
#4909 = CARTESIAN_POINT ( 'NONE',  ( -33.50952539253209039, -41.64595657058005429, -13.38988768305012123 ) ) ;
#4911 = EDGE_LOOP ( 'NONE', ( #11862, #14117, #7063, #3790, #9740 ) ) ;
#4912 = EDGE_CURVE ( 'NONE', #3278, #6631, #1208, .T. ) ;
#4913 = CIRCLE ( 'NONE', #3435, 37.50000000000000000 ) ;
#4914 = CARTESIAN_POINT ( 'NONE',  ( -25.29546517631143132, -15.38982603914036140, 57.00231026484397745 ) ) ;
#4915 = ORIENTED_EDGE ( 'NONE', *, *, #14304, .T. ) ;
#4916 = CARTESIAN_POINT ( 'NONE',  ( -32.76014075162859740, 10.68321993080349763, 16.26994987741149856 ) ) ;
#4917 = CARTESIAN_POINT ( 'NONE',  ( -15.49969986081099904, 64.39262100756199914, 30.46206422150100934 ) ) ;
#4918 = DIRECTION ( 'NONE',  ( 1.387778780781445676E-17, -0.9489765674876077250, -0.3153465940190856021 ) ) ;
#4919 = CARTESIAN_POINT ( 'NONE',  ( -19.76762875079388948, -12.05116796486094977, -13.04444617939184248 ) ) ;
#4920 = CARTESIAN_POINT ( 'NONE',  ( -12.87131257180735844, -22.19373785326158099, 56.85231026484400019 ) ) ;
#4921 = CARTESIAN_POINT ( 'NONE',  ( 2.734184828063399575, -40.49459960338367637, -13.26621881384550861 ) ) ;
#4922 = ORIENTED_EDGE ( 'NONE', *, *, #4318, .T. ) ;
#4923 = ORIENTED_EDGE ( 'NONE', *, *, #8362, .F. ) ;
#4924 = EDGE_LOOP ( 'NONE', ( #4314, #13950, #14402, #6036 ) ) ;
#4925 = EDGE_CURVE ( 'NONE', #7427, #2588, #11539, .T. ) ;
#4926 = LINE ( 'NONE', #35, #12269 ) ;
#4927 = ORIENTED_EDGE ( 'NONE', *, *, #10780, .T. ) ;
#4928 = EDGE_CURVE ( 'NONE', #11333, #10194, #7721, .T. ) ;
#4929 = DIRECTION ( 'NONE',  ( 8.018662683283438208E-16, -5.975035461963189015E-16, -1.000000000000000000 ) ) ;
#4930 = CIRCLE ( 'NONE', #10284, 9.974999999999999645 ) ;
#4931 = DIRECTION ( 'NONE',  ( -8.018662683283438208E-16, 5.975035461963189015E-16, 1.000000000000000000 ) ) ;
#4932 = LINE ( 'NONE', #351, #7772 ) ;
#4933 = VECTOR ( 'NONE', #2545, 1000.000000000000114 ) ;
#4934 = CARTESIAN_POINT ( 'NONE',  ( -23.68291657637574232, -19.21137664199072148, 54.00231026484399166 ) ) ;
#4936 = FACE_OUTER_BOUND ( 'NONE', #990, .T. ) ;
#4935 = CARTESIAN_POINT ( 'NONE',  ( -7.660032944547864986, -48.43376236753701392, -3.904225615250556114 ) ) ;
#4937 = ORIENTED_EDGE ( 'NONE', *, *, #38, .F. ) ;
#4938 = LINE ( 'NONE', #358, #1906 ) ;
#4939 = CYLINDRICAL_SURFACE ( 'NONE', #5209, 5.250000000000000888 ) ;
#4940 = ORIENTED_EDGE ( 'NONE', *, *, #13383, .F. ) ;
#4941 = VERTEX_POINT ( 'NONE', #8269 ) ;
#4942 = CARTESIAN_POINT ( 'NONE',  ( 21.86105357425719475, -27.43463325034647937, 27.44097769609280846 ) ) ;
#4943 = EDGE_CURVE ( 'NONE', #6725, #11422, #10486, .T. ) ;
#4944 = CARTESIAN_POINT ( 'NONE',  ( -16.02267528388033213, -36.50737899243799944, 57.00231026484399877 ) ) ;
#4945 = EDGE_LOOP ( 'NONE', ( #12799, #6285, #12300, #4873, #3617, #6958 ) ) ;
#4946 = CARTESIAN_POINT ( 'NONE',  ( -16.73644428586259636, -23.40541355628490550, 57.00231026484399166 ) ) ;
#4947 = EDGE_CURVE ( 'NONE', #10177, #9929, #3504, .T. ) ;
#4948 = CIRCLE ( 'NONE', #9077, 0.2000000000000012046 ) ;
#4949 = AXIS2_PLACEMENT_3D ( 'NONE', #7488, #1463, #14459 ) ;
#4950 = AXIS2_PLACEMENT_3D ( 'NONE', #12225, #2739, #9778 ) ;
#4951 = CIRCLE ( 'NONE', #14952, 2.500000000000002220 ) ;
#4952 = CARTESIAN_POINT ( 'NONE',  ( -15.49969986081092088, -13.50737899243822504, 56.85231026484398598 ) ) ;
#4953 = CARTESIAN_POINT ( 'NONE',  ( -15.16333526000374832, -10.64029123852186487, 51.25231026484399166 ) ) ;
#4954 = DIRECTION ( 'NONE',  ( 0.000000000000000000, 1.369518533665900312E-16, -1.000000000000000000 ) ) ;
#4955 = CARTESIAN_POINT ( 'NONE',  ( 6.045543233663400073, 20.99262100756200056, 16.16206422150100153 ) ) ;
#4956 = ORIENTED_EDGE ( 'NONE', *, *, #8205, .T. ) ;
#4957 = DIRECTION ( 'NONE',  ( -0.7953815700667019595, -0.6061090314442014737, -2.756373558169989438E-16 ) ) ;
#4958 = PLANE ( 'NONE',  #8753 ) ;
#4959 = VERTEX_POINT ( 'NONE', #10467 ) ;
#4960 = VECTOR ( 'NONE', #926, 1000.000000000000114 ) ;
#4961 = EDGE_CURVE ( 'NONE', #6605, #14388, #8162, .T. ) ;
#4963 = EDGE_CURVE ( 'NONE', #11221, #7892, #9233, .T. ) ;
#4962 = DIRECTION ( 'NONE',  ( -8.018662683283438208E-16, 5.975035461963189015E-16, 1.000000000000000000 ) ) ;
#4964 = SURFACE_STYLE_FILL_AREA ( #11917 ) ;
#4965 = ORIENTED_EDGE ( 'NONE', *, *, #10247, .F. ) ;
#4966 = DIRECTION ( 'NONE',  ( -8.018662683283438208E-16, 5.975035461963189015E-16, 1.000000000000000000 ) ) ;
#4967 = ORIENTED_EDGE ( 'NONE', *, *, #10174, .T. ) ;
#4968 = DIRECTION ( 'NONE',  ( -0.5975035461963188466, -0.8018662683283439563, 0.000000000000000000 ) ) ;
#4969 = DIRECTION ( 'NONE',  ( -0.9320450512859430603, 0.1645000119736390876, -0.3228494516551893012 ) ) ;
#4970 = CARTESIAN_POINT ( 'NONE',  ( -20.69940085690220144, -18.30574950243923027, 57.00231026484397745 ) ) ;
#4971 = ADVANCED_FACE ( 'NONE', ( #4579 ), #5860, .T. ) ;
#4972 = VECTOR ( 'NONE', #10553, 1000.000000000000227 ) ;
#4973 = DIRECTION ( 'NONE',  ( 0.000000000000000000, -1.000000000000000000, -1.224646799147350002E-16 ) ) ;
#4974 = CARTESIAN_POINT ( 'NONE',  ( -15.49969986081099727, 20.99262100756199700, 39.83706422150100224 ) ) ;
#4975 = ORIENTED_EDGE ( 'NONE', *, *, #8399, .T. ) ;
#4976 = CARTESIAN_POINT ( 'NONE',  ( -13.81224214977857123, -23.33861042463823665, 56.85231026484400019 ) ) ;
#4977 = CARTESIAN_POINT ( 'NONE',  ( -9.002116193859002635, -10.70790913352571927, 56.85231026484400019 ) ) ;
#4978 = DIRECTION ( 'NONE',  ( -8.018662683283438208E-16, 5.975035461963189015E-16, 1.000000000000000000 ) ) ;
#4979 = ORIENTED_EDGE ( 'NONE', *, *, #3185, .T. ) ;
#4980 = DIRECTION ( 'NONE',  ( 8.018662683283438208E-16, -5.975035461963189015E-16, -1.000000000000000000 ) ) ;
#4981 = ADVANCED_FACE ( 'NONE', ( #701 ), #988, .T. ) ;
#4982 = EDGE_CURVE ( 'NONE', #11942, #12659, #14980, .T. ) ;
#4983 = VERTEX_POINT ( 'NONE', #3428 ) ;
#4985 = ORIENTED_EDGE ( 'NONE', *, *, #14035, .T. ) ;
#4984 = DIRECTION ( 'NONE',  ( 1.000000000000000000, 9.973326722932540411E-16, 9.491043554366112247E-16 ) ) ;
#4986 = ORIENTED_EDGE ( 'NONE', *, *, #12189, .F. ) ;
#4987 = AXIS2_PLACEMENT_3D ( 'NONE', #3506, #6090, #4735 ) ;
#4988 = EDGE_CURVE ( 'NONE', #5736, #700, #8004, .T. ) ;
#4989 = DIRECTION ( 'NONE',  ( -0.9931883319083343320, 0.1165201156931299220, 0.000000000000000000 ) ) ;
#4990 = EDGE_LOOP ( 'NONE', ( #10966, #5441 ) ) ;
#4991 = FACE_OUTER_BOUND ( 'NONE', #3330, .T. ) ;
#4992 = AXIS2_PLACEMENT_3D ( 'NONE', #3097, #13363, #6455 ) ;
#4993 = DIRECTION ( 'NONE',  ( -8.018662683283438208E-16, 5.975035461963189015E-16, 1.000000000000000000 ) ) ;
#4994 = CARTESIAN_POINT ( 'NONE',  ( -18.47333776534164684, -10.11719227462029735, -13.17042849143727778 ) ) ;
#4995 = EDGE_CURVE ( 'NONE', #5453, #8707, #15119, .T. ) ;
#4996 = VECTOR ( 'NONE', #5264, 1000.000000000000114 ) ;
#4997 = FACE_OUTER_BOUND ( 'NONE', #7873, .T. ) ;
#4998 = FACE_OUTER_BOUND ( 'NONE', #5811, .T. ) ;
#4999 = ORIENTED_EDGE ( 'NONE', *, *, #593, .F. ) ;
#5000 = CARTESIAN_POINT ( 'NONE',  ( -15.49969986081099904, 71.39262100756199914, 17.38382956928560219 ) ) ;
#5001 = AXIS2_PLACEMENT_3D ( 'NONE', #5506, #13699, #999 ) ;
#5002 = ORIENTED_EDGE ( 'NONE', *, *, #7037, .T. ) ;
#5003 = ORIENTED_EDGE ( 'NONE', *, *, #9701, .F. ) ;
#5004 = CARTESIAN_POINT ( 'NONE',  ( -15.27714973199592485, -94.62907795360041519, -10.37839032168656672 ) ) ;
#5005 = ORIENTED_EDGE ( 'NONE', *, *, #2055, .F. ) ;
#5006 = ORIENTED_EDGE ( 'NONE', *, *, #13187, .F. ) ;
#5007 = FACE_OUTER_BOUND ( 'NONE', #12198, .T. ) ;
#5008 = CARTESIAN_POINT ( 'NONE',  ( -24.85752488709640318, -10.05314452190415508, 54.00231026484397745 ) ) ;
#5009 = VECTOR ( 'NONE', #7625, 1000.000000000000000 ) ;
#5010 = DIRECTION ( 'NONE',  ( 0.000000000000000000, -1.000000000000000000, -1.224646799147350002E-16 ) ) ;
#5011 = FACE_OUTER_BOUND ( 'NONE', #4990, .T. ) ;
#5012 = EDGE_CURVE ( 'NONE', #4831, #14554, #10388, .T. ) ;
#5013 = DIRECTION ( 'NONE',  ( 0.000000000000000000, 0.000000000000000000, 1.000000000000000000 ) ) ;
#5014 = AXIS2_PLACEMENT_3D ( 'NONE', #1989, #4437, #690 ) ;
#5016 = LINE ( 'NONE', #1790, #9623 ) ;
#5015 = CARTESIAN_POINT ( 'NONE',  ( -15.61203582816999713, -107.9994814593942607, -7.057848339359948042 ) ) ;
#5017 = VERTEX_POINT ( 'NONE', #5939 ) ;
#5018 = CARTESIAN_POINT ( 'NONE',  ( 2.500300139188999626, -46.50737899243799944, -7.997689735156003010 ) ) ;
#5019 = DIRECTION ( 'NONE',  ( 0.000000000000000000, 1.000000000000000000, 1.224646799147350002E-16 ) ) ;
#5020 = EDGE_LOOP ( 'NONE', ( #13892, #9003, #10636, #6944 ) ) ;
#5021 = ORIENTED_EDGE ( 'NONE', *, *, #13298, .F. ) ;
#5022 = PLANE ( 'NONE',  #9321 ) ;
#5023 = VERTEX_POINT ( 'NONE', #12999 ) ;
#5024 = CARTESIAN_POINT ( 'NONE',  ( -15.49969986081099904, -13.50737899243800122, 6.712064221500998684 ) ) ;
#5025 = DIRECTION ( 'NONE',  ( -8.018662683283439195E-16, 5.975035461963190001E-16, 1.000000000000000000 ) ) ;
#5026 = EDGE_CURVE ( 'NONE', #11857, #2792, #8238, .T. ) ;
#5027 = CARTESIAN_POINT ( 'NONE',  ( -9.226714359780459063, -21.29551127497027707, 56.47371171714189586 ) ) ;
#5028 = LINE ( 'NONE', #14205, #883 ) ;
#5029 = LINE ( 'NONE', #440, #5448 ) ;
#5030 = EDGE_CURVE ( 'NONE', #14164, #17, #11839, .T. ) ;
#5031 = ORIENTED_EDGE ( 'NONE', *, *, #8998, .F. ) ;
#5032 = CARTESIAN_POINT ( 'NONE',  ( -16.32149003149045896, -5.473954385499117947, 57.00231026484397745 ) ) ;
#5033 = CARTESIAN_POINT ( 'NONE',  ( -7.985436018829467741, -20.06759727486528533, 54.00231026484400587 ) ) ;
#5034 = ORIENTED_EDGE ( 'NONE', *, *, #3225, .T. ) ;
#5035 = DIRECTION ( 'NONE',  ( 0.000000000000000000, -1.000000000000000000, -1.224646799147350002E-16 ) ) ;
#5036 = LINE ( 'NONE', #12221, #1153 ) ;
#5037 = ORIENTED_EDGE ( 'NONE', *, *, #2614, .F. ) ;
#5038 = AXIS2_PLACEMENT_3D ( 'NONE', #9765, #12069, #2580 ) ;
#5039 = DIRECTION ( 'NONE',  ( -8.018662683283439195E-16, 5.975035461963190001E-16, 1.000000000000000000 ) ) ;
#5040 = VERTEX_POINT ( 'NONE', #4807 ) ;
#5041 = LINE ( 'NONE', #5113, #4707 ) ;
#5042 = DIRECTION ( 'NONE',  ( 0.000000000000000000, 0.000000000000000000, 1.000000000000000000 ) ) ;
#5043 = ADVANCED_FACE ( 'NONE', ( #3734, #9394 ), #8389, .T. ) ;
#5044 = CARTESIAN_POINT ( 'NONE',  ( -7.516520390631877824, -48.95538363176652297, 18.97731922801482440 ) ) ;
#5045 = ADVANCED_FACE ( 'NONE', ( #8467 ), #379, .F. ) ;
#5046 = CIRCLE ( 'NONE', #13598, 3.250000000000002665 ) ;
#5047 = CARTESIAN_POINT ( 'NONE',  ( 17.56619466861842227, -29.98873796865039765, 6.521841211496442803 ) ) ;
#5048 = EDGE_CURVE ( 'NONE', #5628, #7811, #10617, .T. ) ;
#5049 = EDGE_LOOP ( 'NONE', ( #14582, #12983, #7717, #3897 ) ) ;
#5050 = CARTESIAN_POINT ( 'NONE',  ( -7.768786321151917917, -46.58155647109239084, -17.19222724300273342 ) ) ;
#5051 = DIRECTION ( 'NONE',  ( -8.018662683283438208E-16, 5.975035461963189015E-16, 1.000000000000000000 ) ) ;
#5052 = ORIENTED_EDGE ( 'NONE', *, *, #7570, .T. ) ;
#5053 = DIRECTION ( 'NONE',  ( 0.8357240892757724637, 0.5491495666976171641, 3.420201433256690644E-16 ) ) ;
#5054 = VERTEX_POINT ( 'NONE', #8311 ) ;
#5056 = ORIENTED_EDGE ( 'NONE', *, *, #747, .F. ) ;
#5055 = CARTESIAN_POINT ( 'NONE',  ( -33.49969986081099904, -51.00737899243799944, -13.39525803434800011 ) ) ;
#5057 = EDGE_CURVE ( 'NONE', #14532, #11915, #4382, .T. ) ;
#5058 = ORIENTED_EDGE ( 'NONE', *, *, #12976, .F. ) ;
#5059 = CYLINDRICAL_SURFACE ( 'NONE', #1770, 0.2500000000000014433 ) ;
#5060 = CIRCLE ( 'NONE', #13367, 0.2000000000000012046 ) ;
#5061 = ORIENTED_EDGE ( 'NONE', *, *, #13777, .F. ) ;
#5062 = CARTESIAN_POINT ( 'NONE',  ( -33.05408098453766996, 8.544173770627832454, 16.94260638916070150 ) ) ;
#5063 = VECTOR ( 'NONE', #3543, 1000.000000000000000 ) ;
#5064 = EDGE_CURVE ( 'NONE', #1451, #13944, #14368, .T. ) ;
#5065 = CARTESIAN_POINT ( 'NONE',  ( -12.90403152030055800, -3.849063734251706670, 61.62346604207912293 ) ) ;
#5066 = APPLICATION_PROTOCOL_DEFINITION ( 'draft international standard', 'automotive_design', 1998, #107 ) ;
#5067 = EDGE_CURVE ( 'NONE', #1266, #12240, #8281, .T. ) ;
#5068 = PLANE ( 'NONE',  #456 ) ;
#5069 = DIRECTION ( 'NONE',  ( 0.000000000000000000, -1.000000000000000000, -1.224646799147350002E-16 ) ) ;
#5070 = LINE ( 'NONE', #12329, #3963 ) ;
#5071 = VERTEX_POINT ( 'NONE', #12927 ) ;
#5072 = CARTESIAN_POINT ( 'NONE',  ( -15.49969986081099194, -110.0146955301539151, -11.10449286955627102 ) ) ;
#5073 = ORIENTED_EDGE ( 'NONE', *, *, #3030, .F. ) ;
#5074 = VECTOR ( 'NONE', #3032, 1000.000000000000000 ) ;
#5075 = EDGE_LOOP ( 'NONE', ( #5141, #14047, #7371, #207 ) ) ;
#5076 = DIRECTION ( 'NONE',  ( 8.018662683283438208E-16, -5.975035461963189015E-16, -1.000000000000000000 ) ) ;
#5077 = ORIENTED_EDGE ( 'NONE', *, *, #2819, .F. ) ;
#5078 = ORIENTED_EDGE ( 'NONE', *, *, #3431, .T. ) ;
#5079 = DIRECTION ( 'NONE',  ( 9.943800201373337757E-16, -0.1872998510044509290, -0.9823027872370669877 ) ) ;
#5080 = AXIS2_PLACEMENT_3D ( 'NONE', #13388, #2896, #14677 ) ;
#5081 = DIRECTION ( 'NONE',  ( 1.000000000000000000, 0.000000000000000000, 1.224646799147350002E-16 ) ) ;
#5082 = AXIS2_PLACEMENT_3D ( 'NONE', #9763, #14428, #3948 ) ;
#5083 = FACE_OUTER_BOUND ( 'NONE', #5291, .T. ) ;
#5084 = APPLICATION_CONTEXT ( 'automotive_design' ) ;
#5085 = DIRECTION ( 'NONE',  ( 0.5975035461963189576, 0.8018662683283437342, 0.000000000000000000 ) ) ;
#5087 = CARTESIAN_POINT ( 'NONE',  ( -15.49969986081099904, 22.99262100756200411, 8.587064221501004013 ) ) ;
#5086 = CARTESIAN_POINT ( 'NONE',  ( -15.49969986081092088, -13.50737899243822504, 56.85231026484398598 ) ) ;
#5088 = ORIENTED_EDGE ( 'NONE', *, *, #8757, .F. ) ;
#5089 = CARTESIAN_POINT ( 'NONE',  ( -18.09969986081099336, -110.0468591183650915, -10.12107724339962722 ) ) ;
#5090 = ORIENTED_EDGE ( 'NONE', *, *, #1430, .F. ) ;
#5091 = VECTOR ( 'NONE', #7980, 1000.000000000000000 ) ;
#5092 = DIRECTION ( 'NONE',  ( -1.000000000000000000, 1.499759782661860071E-32, -1.224646799147350002E-16 ) ) ;
#5093 = ORIENTED_EDGE ( 'NONE', *, *, #6985, .T. ) ;
#5094 = ORIENTED_EDGE ( 'NONE', *, *, #4402, .T. ) ;
#5095 = CIRCLE ( 'NONE', #6530, 6.250000000000001776 ) ;
#5096 = VECTOR ( 'NONE', #103, 999.9999999999998863 ) ;
#5097 = DIRECTION ( 'NONE',  ( 0.000000000000000000, 1.224646799147350002E-16, -1.000000000000000000 ) ) ;
#5098 = VERTEX_POINT ( 'NONE', #1513 ) ;
#5099 = ADVANCED_FACE ( 'NONE', ( #14139 ), #3660, .F. ) ;
#5100 = EDGE_CURVE ( 'NONE', #8254, #12536, #12192, .T. ) ;
#5101 = CARTESIAN_POINT ( 'NONE',  ( -8.194314379747492438, -16.94868586237404529, 57.00231026484399166 ) ) ;
#5102 = LINE ( 'NONE', #11061, #6769 ) ;
#5103 = DIRECTION ( 'NONE',  ( 0.000000000000000000, -0.05233595624293968518, -0.9986295347545740553 ) ) ;
#5104 = DIRECTION ( 'NONE',  ( 1.000000000000000000, 1.201369187114119994E-15, 9.616040805000176517E-16 ) ) ;
#5105 = ORIENTED_EDGE ( 'NONE', *, *, #14953, .F. ) ;
#5106 = FACE_OUTER_BOUND ( 'NONE', #8625, .T. ) ;
#5107 = DIRECTION ( 'NONE',  ( 0.000000000000000000, -2.168404344971007882E-16, 1.000000000000000000 ) ) ;
#5108 = ORIENTED_EDGE ( 'NONE', *, *, #11580, .T. ) ;
#5109 = CARTESIAN_POINT ( 'NONE',  ( 21.99848766979616599, -23.77809160205145034, 24.63628493690049481 ) ) ;
#5110 = ORIENTED_EDGE ( 'NONE', *, *, #12681, .F. ) ;
#5111 = CARTESIAN_POINT ( 'NONE',  ( -5.499699860810997265, -46.50737899243799944, -5.497689735156003010 ) ) ;
#5112 = ORIENTED_EDGE ( 'NONE', *, *, #10743, .T. ) ;
#5113 = CARTESIAN_POINT ( 'NONE',  ( -7.499699860810999041, -44.50737899243799944, -109.5506571639849938 ) ) ;
#5114 = EDGE_CURVE ( 'NONE', #3941, #12614, #6011, .T. ) ;
#5115 = DIRECTION ( 'NONE',  ( -8.018662683283438208E-16, 5.975035461963189015E-16, 1.000000000000000000 ) ) ;
#5116 = VECTOR ( 'NONE', #3771, 1000.000000000000000 ) ;
#5117 = CARTESIAN_POINT ( 'NONE',  ( -7.752363797594753692, -48.01475789269077410, 17.50266728317557963 ) ) ;
#5118 = DIRECTION ( 'NONE',  ( -1.000000000000000000, 0.000000000000000000, 0.000000000000000000 ) ) ;
#5119 = CARTESIAN_POINT ( 'NONE',  ( 22.00030013918900096, -27.00737899243800300, 39.96206422150099513 ) ) ;
#5120 = ORIENTED_EDGE ( 'NONE', *, *, #3814, .F. ) ;
#5121 = CARTESIAN_POINT ( 'NONE',  ( -7.705135643603000517, -46.32754971434033564, -17.17871339279434295 ) ) ;
#5122 = CARTESIAN_POINT ( 'NONE',  ( -2.216578225681298697, -31.14135358865360104, 59.28069236156870403 ) ) ;
#5123 = ORIENTED_EDGE ( 'NONE', *, *, #12518, .F. ) ;
#5124 = DIRECTION ( 'NONE',  ( -9.912705577010322591E-16, 0.1872998510044552312, 0.9823027872370662106 ) ) ;
#5125 = ORIENTED_EDGE ( 'NONE', *, *, #10846, .F. ) ;
#5127 = ORIENTED_EDGE ( 'NONE', *, *, #650, .F. ) ;
#5126 = CARTESIAN_POINT ( 'NONE',  ( -7.754796638793765240, -46.50763592918296752, 17.00313569000094560 ) ) ;
#5128 = ORIENTED_EDGE ( 'NONE', *, *, #354, .F. ) ;
#5129 = VECTOR ( 'NONE', #8770, 1000.000000000000000 ) ;
#5130 = ADVANCED_FACE ( 'NONE', ( #7314 ), #219, .T. ) ;
#5131 = CARTESIAN_POINT ( 'NONE',  ( -5.499699860810998153, -46.50737899243799944, -8.497689735156003010 ) ) ;
#5132 = ORIENTED_EDGE ( 'NONE', *, *, #12664, .F. ) ;
#5133 = EDGE_CURVE ( 'NONE', #6753, #7373, #957, .T. ) ;
#5134 = DIRECTION ( 'NONE',  ( 0.9635179096299403279, 0.05012965580939313798, 0.2629073133839797682 ) ) ;
#5135 = DIRECTION ( 'NONE',  ( 0.000000000000000000, 1.000000000000000000, 1.224646799147350002E-16 ) ) ;
#5136 = CARTESIAN_POINT ( 'NONE',  ( -12.81093390292742740, -9.898980784960722090, -13.99768973515600301 ) ) ;
#5137 = CARTESIAN_POINT ( 'NONE',  ( -7.500924733540946576, -44.35427680771954329, 45.77981586235881650 ) ) ;
#5138 = DIRECTION ( 'NONE',  ( -1.000000000000000000, 0.000000000000000000, 0.000000000000000000 ) ) ;
#5139 = VERTEX_POINT ( 'NONE', #10847 ) ;
#5140 = DIRECTION ( 'NONE',  ( 0.000000000000000000, 0.1872998510044689147, 0.9823027872370635460 ) ) ;
#5141 = ORIENTED_EDGE ( 'NONE', *, *, #12469, .T. ) ;
#5142 = ORIENTED_EDGE ( 'NONE', *, *, #4317, .F. ) ;
#5143 = EDGE_CURVE ( 'NONE', #36, #14829, #4782, .T. ) ;
#5144 = CARTESIAN_POINT ( 'NONE',  ( -15.34686821047329808, -23.48120812104550481, 56.85231026484400019 ) ) ;
#5145 = EDGE_CURVE ( 'NONE', #6476, #11680, #5423, .T. ) ;
#5146 = ORIENTED_EDGE ( 'NONE', *, *, #10557, .T. ) ;
#5147 = CARTESIAN_POINT ( 'NONE',  ( -12.75555302399369850, -9.928823230469003391, -13.18819869426426727 ) ) ;
#5148 = DIRECTION ( 'NONE',  ( 0.5975035461963189576, 0.8018662683283437342, 0.000000000000000000 ) ) ;
#5149 = CARTESIAN_POINT ( 'NONE',  ( -14.95642007119156425, -3.547184613301258782, 57.00231026484397745 ) ) ;
#5151 = DIRECTION ( 'NONE',  ( 0.5975035461963189576, 0.8018662683283437342, 0.000000000000000000 ) ) ;
#5150 = DIRECTION ( 'NONE',  ( -8.018662683283439195E-16, 5.975035461963190001E-16, 1.000000000000000000 ) ) ;
#5152 = VERTEX_POINT ( 'NONE', #6235 ) ;
#5153 = CARTESIAN_POINT ( 'NONE',  ( 2.500300139189002291, -46.50737899243799944, -8.497689735156001234 ) ) ;
#5154 = EDGE_LOOP ( 'NONE', ( #5783, #11649, #12121, #3903 ) ) ;
#5155 = CARTESIAN_POINT ( 'NONE',  ( -15.19545581216392627, -5.437764035151672282, 56.85231026484398598 ) ) ;
#5156 = ORIENTED_EDGE ( 'NONE', *, *, #12189, .T. ) ;
#5157 = EDGE_LOOP ( 'NONE', ( #4066, #442, #13026, #7199 ) ) ;
#5158 = VECTOR ( 'NONE', #15115, 999.9999999999998863 ) ;
#5159 = DIRECTION ( 'NONE',  ( 0.5975035461963189576, 0.8018662683283437342, 0.000000000000000000 ) ) ;
#5160 = EDGE_CURVE ( 'NONE', #118, #10152, #3957, .T. ) ;
#5161 = ORIENTED_EDGE ( 'NONE', *, *, #8209, .F. ) ;
#5162 = LINE ( 'NONE', #8749, #9338 ) ;
#5163 = ADVANCED_FACE ( 'NONE', ( #9773, #4260 ), #12371, .T. ) ;
#5164 = CARTESIAN_POINT ( 'NONE',  ( 4.685129763540130554, 6.083222336766384686, 18.77103779417431895 ) ) ;
#5165 = CARTESIAN_POINT ( 'NONE',  ( -20.61091276329630162, -106.9682996518086497, -7.149495196850712553 ) ) ;
#5166 = VECTOR ( 'NONE', #12635, 1000.000000000000000 ) ;
#5167 = LINE ( 'NONE', #8679, #14597 ) ;
#5168 = EDGE_CURVE ( 'NONE', #4749, #7809, #1307, .T. ) ;
#5169 = CARTESIAN_POINT ( 'NONE',  ( -10.07958688850791162, -7.521259601090221736, 56.85231026484398598 ) ) ;
#5170 = CARTESIAN_POINT ( 'NONE',  ( -31.79969986081099975, 3.992621007561997892, 24.16206422150099797 ) ) ;
#5171 = EDGE_LOOP ( 'NONE', ( #13803, #318 ) ) ;
#5172 = CARTESIAN_POINT ( 'NONE',  ( -15.49969986081099194, -27.00737899243800300, 19.50231026484399877 ) ) ;
#5173 = CARTESIAN_POINT ( 'NONE',  ( -15.49969986081092088, -13.50737899243822504, 56.85231026484398598 ) ) ;
#5174 = ORIENTED_EDGE ( 'NONE', *, *, #266, .T. ) ;
#5175 = AXIS2_PLACEMENT_3D ( 'NONE', #1626, #11110, #559 ) ;
#5176 = CARTESIAN_POINT ( 'NONE',  ( 21.91129973042178491, -25.02583635234388026, 26.79684541854832247 ) ) ;
#5177 = ORIENTED_EDGE ( 'NONE', *, *, #2672, .T. ) ;
#5178 = CARTESIAN_POINT ( 'NONE',  ( -33.49969986081099904, -51.00737899243799944, 52.39987856403599409 ) ) ;
#5179 = ORIENTED_EDGE ( 'NONE', *, *, #288, .F. ) ;
#5180 = CARTESIAN_POINT ( 'NONE',  ( -15.61203582817000068, -106.9748017008338365, -5.104852750214476487 ) ) ;
#5181 = CONICAL_SURFACE ( 'NONE', #11770, 1.750000000000000666, 0.2709468503384208082 ) ;
#5182 = AXIS2_PLACEMENT_3D ( 'NONE', #5277, #8715, #10085 ) ;
#5183 = LINE ( 'NONE', #8996, #12271 ) ;
#5184 = CARTESIAN_POINT ( 'NONE',  ( -7.886584594865180264, -46.96511696614940234, -3.039951761444701361 ) ) ;
#5185 = VECTOR ( 'NONE', #4107, 1000.000000000000000 ) ;
#5186 = VECTOR ( 'NONE', #3132, 1000.000000000000000 ) ;
#5187 = AXIS2_PLACEMENT_3D ( 'NONE', #7471, #4040, #3810 ) ;
#5188 = EDGE_CURVE ( 'NONE', #8489, #11739, #446, .T. ) ;
#5189 = VECTOR ( 'NONE', #14299, 999.9999999999998863 ) ;
#5190 = CARTESIAN_POINT ( 'NONE',  ( 15.85054478794847554, -29.85571724108492120, 3.634072666459030820 ) ) ;
#5191 = CARTESIAN_POINT ( 'NONE',  ( 13.85920135429429934, -27.00737899243800300, 20.96206422150100224 ) ) ;
#5192 = VERTEX_POINT ( 'NONE', #5329 ) ;
#5193 = CARTESIAN_POINT ( 'NONE',  ( -13.96026682931439211, -23.36287344688023992, 57.00231026484399166 ) ) ;
#5194 = CARTESIAN_POINT ( 'NONE',  ( -15.57469986081099478, -26.50737899243800300, 56.85231026484400019 ) ) ;
#5195 = ORIENTED_EDGE ( 'NONE', *, *, #2438, .F. ) ;
#5196 = EDGE_LOOP ( 'NONE', ( #3635, #12276, #4408, #3198 ) ) ;
#5198 = EDGE_LOOP ( 'NONE', ( #7273, #5915 ) ) ;
#5197 = CARTESIAN_POINT ( 'NONE',  ( -34.85309570014907621, -38.58518656690294790, -12.61778470598987312 ) ) ;
#5199 = ORIENTED_EDGE ( 'NONE', *, *, #3469, .T. ) ;
#5200 = CARTESIAN_POINT ( 'NONE',  ( -23.49969986081099904, -19.50737899243800300, 6.712064221500998684 ) ) ;
#5201 = DIRECTION ( 'NONE',  ( 1.000000000000000000, 1.201369187114119994E-15, 9.616040805000176517E-16 ) ) ;
#5202 = ORIENTED_EDGE ( 'NONE', *, *, #10459, .F. ) ;
#5203 = CIRCLE ( 'NONE', #806, 9.974999999999999645 ) ;
#5204 = LINE ( 'NONE', #5501, #2258 ) ;
#5205 = CARTESIAN_POINT ( 'NONE',  ( -33.11203844197629564, 8.260196310773684658, 17.08384978814601141 ) ) ;
#5206 = CARTESIAN_POINT ( 'NONE',  ( -15.49969986081099904, -13.50737899243800122, 6.712064221500998684 ) ) ;
#5207 = CARTESIAN_POINT ( 'NONE',  ( -15.49969986081099904, -13.50737899243800122, 56.85231026484400019 ) ) ;
#5208 = EDGE_CURVE ( 'NONE', #13485, #1568, #13521, .T. ) ;
#5209 = AXIS2_PLACEMENT_3D ( 'NONE', #12055, #5019, #14347 ) ;
#5210 = VECTOR ( 'NONE', #2924, 1000.000000000000114 ) ;
#5211 = CARTESIAN_POINT ( 'NONE',  ( -16.38999062866295020, -11.44100962838991364, 51.00231026484399166 ) ) ;
#5212 = EDGE_CURVE ( 'NONE', #11184, #9718, #3031, .T. ) ;
#5213 = ORIENTED_EDGE ( 'NONE', *, *, #4624, .T. ) ;
#5214 = CARTESIAN_POINT ( 'NONE',  ( -19.68577560955674954, -20.41303028871448788, 57.00231026484397745 ) ) ;
#5215 = VECTOR ( 'NONE', #11216, 1000.000000000000000 ) ;
#5216 = AXIS2_PLACEMENT_3D ( 'NONE', #12293, #8832, #1814 ) ;
#5217 = ORIENTED_EDGE ( 'NONE', *, *, #14933, .T. ) ;
#5218 = CARTESIAN_POINT ( 'NONE',  ( -3.499699860810999041, -57.00737899243800655, 55.03046811182510112 ) ) ;
#5220 = ORIENTED_EDGE ( 'NONE', *, *, #14468, .T. ) ;
#5219 = CARTESIAN_POINT ( 'NONE',  ( -7.498763094504910853, -44.75646166653845626, -7.292659265823624004 ) ) ;
#5221 = VERTEX_POINT ( 'NONE', #13597 ) ;
#5222 = CARTESIAN_POINT ( 'NONE',  ( -18.54556661251663030, -20.98627902725976213, 56.85231026484398598 ) ) ;
#5223 = ORIENTED_EDGE ( 'NONE', *, *, #11984, .F. ) ;
#5224 = CARTESIAN_POINT ( 'NONE',  ( -1.508527451664999575, -47.37340439622243338, -3.997689735156000790 ) ) ;
#5225 = CIRCLE ( 'NONE', #11326, 1.750000000000000666 ) ;
#5226 = DIRECTION ( 'NONE',  ( 1.000000000000000000, 0.000000000000000000, 0.000000000000000000 ) ) ;
#5227 = DIRECTION ( 'NONE',  ( -0.9183863840214729901, -0.3956847857120157075, -4.999999999999999402E-16 ) ) ;
#5228 = EDGE_CURVE ( 'NONE', #2134, #572, #9334, .T. ) ;
#5229 = EDGE_CURVE ( 'NONE', #8291, #14012, #550, .T. ) ;
#5230 = CIRCLE ( 'NONE', #12322, 23.00000000000000000 ) ;
#5232 = CARTESIAN_POINT ( 'NONE',  ( -35.96525066421718009, 5.948560758909089863, 18.92081361401057649 ) ) ;
#5231 = CARTESIAN_POINT ( 'NONE',  ( 13.85920135429429934, -27.00737899243800300, 8.462064221501000461 ) ) ;
#5233 = EDGE_CURVE ( 'NONE', #11156, #2347, #10058, .T. ) ;
#5234 = ORIENTED_EDGE ( 'NONE', *, *, #12244, .F. ) ;
#5235 = LINE ( 'NONE', #427, #8978 ) ;
#5236 = ORIENTED_EDGE ( 'NONE', *, *, #9575, .T. ) ;
#5237 = PLANE ( 'NONE',  #7149 ) ;
#5238 = ORIENTED_EDGE ( 'NONE', *, *, #1315, .T. ) ;
#5239 = ORIENTED_EDGE ( 'NONE', *, *, #7736, .T. ) ;
#5240 = VECTOR ( 'NONE', #14599, 999.9999999999998863 ) ;
#5241 = CARTESIAN_POINT ( 'NONE',  ( -23.49969986081100970, -45.03523210613074212, 56.13904046828874073 ) ) ;
#5242 = ORIENTED_EDGE ( 'NONE', *, *, #10015, .T. ) ;
#5243 = ADVANCED_FACE ( 'NONE', ( #14814 ), #6608, .T. ) ;
#5244 = CARTESIAN_POINT ( 'NONE',  ( -14.18877560904499902, -36.61116194625252973, 56.98027335662509074 ) ) ;
#5245 = CARTESIAN_POINT ( 'NONE',  ( -7.758527451664999575, -46.50737899243799944, -5.497689735156000346 ) ) ;
#5246 = CARTESIAN_POINT ( 'NONE',  ( -20.72174206363053273, -106.3077111449690619, -6.767278426752862508 ) ) ;
#5247 = AXIS2_PLACEMENT_3D ( 'NONE', #767, #846, #10013 ) ;
#5248 = CARTESIAN_POINT ( 'NONE',  ( -9.119211481053252299, -21.20735069469006717, 56.45528369196469498 ) ) ;
#5249 = EDGE_CURVE ( 'NONE', #12040, #8177, #3414, .T. ) ;
#5250 = CARTESIAN_POINT ( 'NONE',  ( -23.43263029221230198, -15.01730109988151440, 56.85231026484398598 ) ) ;
#5251 = CARTESIAN_POINT ( 'NONE',  ( -5.499699860811000818, -46.50737899243799944, 19.50231026484399877 ) ) ;
#5252 = ORIENTED_EDGE ( 'NONE', *, *, #3883, .F. ) ;
#5253 = DIRECTION ( 'NONE',  ( 1.000000000000000000, 1.201369187114119994E-15, 9.616040805000176517E-16 ) ) ;
#5254 = CARTESIAN_POINT ( 'NONE',  ( -23.55378106252664239, -12.92169478045303066, 56.85231026484398598 ) ) ;
#5255 = ORIENTED_EDGE ( 'NONE', *, *, #2531, .T. ) ;
#5256 = CARTESIAN_POINT ( 'NONE',  ( 21.88649023383436187, -25.56571653516489206, 27.13259355918092552 ) ) ;
#5257 = CARTESIAN_POINT ( 'NONE',  ( -23.37741044072812713, -11.73331557219068877, 56.85231026484398598 ) ) ;
#5258 = ORIENTED_EDGE ( 'NONE', *, *, #1317, .T. ) ;
#5259 = VECTOR ( 'NONE', #8646, 1000.000000000000000 ) ;
#5260 = EDGE_CURVE ( 'NONE', #4893, #1960, #11519, .T. ) ;
#5261 = CARTESIAN_POINT ( 'NONE',  ( -21.49969986081095996, -67.00737899243799234, -5.497689735156006563 ) ) ;
#5262 = CARTESIAN_POINT ( 'NONE',  ( -18.68395610307571530, -20.92841410781112899, 56.85231026484398598 ) ) ;
#5263 = FACE_OUTER_BOUND ( 'NONE', #8023, .T. ) ;
#5264 = DIRECTION ( 'NONE',  ( -0.8934395198752397294, 0.4491835085186243748, -9.848077530122081084E-16 ) ) ;
#5265 = ORIENTED_EDGE ( 'NONE', *, *, #6658, .F. ) ;
#5266 = DIRECTION ( 'NONE',  ( -8.673617379884027583E-16, 1.000000000000000000, 0.000000000000000000 ) ) ;
#5267 = CARTESIAN_POINT ( 'NONE',  ( -21.89842656004739396, -7.071732433740530510, 57.00231026484397745 ) ) ;
#5268 = EDGE_LOOP ( 'NONE', ( #431, #11313, #6838, #6857 ) ) ;
#5270 = EDGE_LOOP ( 'NONE', ( #9967, #6390, #2528, #8370 ) ) ;
#5269 = DIRECTION ( 'NONE',  ( 0.000000000000000000, -1.000000000000000000, -1.224646799147350002E-16 ) ) ;
#5271 = B_SPLINE_CURVE_WITH_KNOTS ( 'NONE', 3,
 ( #2263, #8058, #15106, #12749, #5543, #11591, #1108, #5766, #4634, #2034 ),
 .UNSPECIFIED., .F., .F.,
 ( 4, 2, 2, 2, 4 ),
 ( 0.005531701047751949943, 0.006113612598919536401, 0.006695524150087122858, 0.007277435701254709316, 0.007859347252422295774 ),
 .UNSPECIFIED. ) ;
#5272 = ORIENTED_EDGE ( 'NONE', *, *, #11015, .T. ) ;
#5273 = DIRECTION ( 'NONE',  ( 1.000000000000000000, 0.000000000000000000, 0.000000000000000000 ) ) ;
#5274 = DIRECTION ( 'NONE',  ( 0.000000000000000000, 0.000000000000000000, 1.000000000000000000 ) ) ;
#5275 = EDGE_CURVE ( 'NONE', #12154, #8967, #10561, .T. ) ;
#5276 = EDGE_CURVE ( 'NONE', #11014, #5496, #5477, .T. ) ;
#5277 = CARTESIAN_POINT ( 'NONE',  ( -15.49969986081099194, -32.00737899243799944, 19.50231026484399166 ) ) ;
#5278 = CARTESIAN_POINT ( 'NONE',  ( -23.41792317787242084, -15.09084496969942535, 56.85231026484398598 ) ) ;
#5279 = AXIS2_PLACEMENT_3D ( 'NONE', #11304, #10071, #14822 ) ;
#5280 = CARTESIAN_POINT ( 'NONE',  ( -15.49969986081099904, 3.992621007561997892, 24.21206422150100224 ) ) ;
#5281 = B_SPLINE_CURVE_WITH_KNOTS ( 'NONE', 3,
 ( #1724, #4028, #8534, #509 ),
 .UNSPECIFIED., .F., .F.,
 ( 4, 4 ),
 ( 0.000000000000000000, 1.000000000000000000 ),
 .UNSPECIFIED. ) ;
#5282 = FACE_OUTER_BOUND ( 'NONE', #13096, .T. ) ;
#5283 = DIRECTION ( 'NONE',  ( 0.000000000000000000, 1.000000000000000000, 1.224646799147350002E-16 ) ) ;
#5284 = CARTESIAN_POINT ( 'NONE',  ( -7.499699860810999930, -44.42675748898079036, 45.89481492690103437 ) ) ;
#5285 = EDGE_LOOP ( 'NONE', ( #2472, #13798, #7989, #10603 ) ) ;
#5286 = CARTESIAN_POINT ( 'NONE',  ( -17.87376992080280758, -22.26666214519964271, 56.85231026484400019 ) ) ;
#5287 = VERTEX_POINT ( 'NONE', #10217 ) ;
#5288 = CARTESIAN_POINT ( 'NONE',  ( -8.194314379747492438, -16.94868586237404529, 56.85231026484400019 ) ) ;
#5290 = ORIENTED_EDGE ( 'NONE', *, *, #5870, .T. ) ;
#5289 = CARTESIAN_POINT ( 'NONE',  ( -18.09969986081091164, -109.9722034095862995, -10.19792577984107318 ) ) ;
#5291 = EDGE_LOOP ( 'NONE', ( #4731, #9413, #6379, #9356 ) ) ;
#5292 = CARTESIAN_POINT ( 'NONE',  ( -15.49969986081099904, -57.00737899243800655, 19.50231026484399877 ) ) ;
#5294 = EDGE_LOOP ( 'NONE', ( #4011, #2796, #14760, #3377 ) ) ;
#5293 = DIRECTION ( 'NONE',  ( -8.018662683283438208E-16, 5.975035461963189015E-16, 1.000000000000000000 ) ) ;
#5295 = CIRCLE ( 'NONE', #12885, 9.974999999999999645 ) ;
#5296 = CARTESIAN_POINT ( 'NONE',  ( -13.24439404687306165, -9.602254296713979898, -13.22085716751162288 ) ) ;
#5297 = EDGE_CURVE ( 'NONE', #12356, #777, #11903, .T. ) ;
#5298 = CARTESIAN_POINT ( 'NONE',  ( -15.49969986081099904, -19.50737899243800300, 24.21206422150100224 ) ) ;
#5299 = PLANE ( 'NONE',  #11448 ) ;
#5300 = CIRCLE ( 'NONE', #14092, 4.499999999999999112 ) ;
#5301 = VECTOR ( 'NONE', #13930, 1000.000000000000114 ) ;
#5303 = CARTESIAN_POINT ( 'NONE',  ( -35.92016838155372938, 5.970170166553522506, 18.89611068059123866 ) ) ;
#5302 = DIRECTION ( 'NONE',  ( -0.1617534816134003905, 0.9868311969055008070, -7.193398003386493154E-16 ) ) ;
#5304 = VERTEX_POINT ( 'NONE', #13895 ) ;
#5305 = CARTESIAN_POINT ( 'NONE',  ( -6.309378268457435546, -9.629413800598410234, 57.00231026484399166 ) ) ;
#5306 = VERTEX_POINT ( 'NONE', #3189 ) ;
#5307 = DIRECTION ( 'NONE',  ( 7.070501591499380254E-17, 1.224646799147350002E-16, -1.000000000000000000 ) ) ;
#5308 = ORIENTED_EDGE ( 'NONE', *, *, #10557, .F. ) ;
#5309 = ORIENTED_EDGE ( 'NONE', *, *, #14539, .T. ) ;
#5310 = LINE ( 'NONE', #9902, #1030 ) ;
#5311 = EDGE_LOOP ( 'NONE', ( #8782, #10943, #1642, #14348 ) ) ;
#5312 = AXIS2_PLACEMENT_3D ( 'NONE', #2502, #8235, #3728 ) ;
#5313 = CARTESIAN_POINT ( 'NONE',  ( -12.19373306175957161, -37.21772783548635744, 56.85708728699461290 ) ) ;
#5314 = EDGE_CURVE ( 'NONE', #1146, #2196, #14469, .T. ) ;
#5315 = AXIS2_PLACEMENT_3D ( 'NONE', #1353, #10456, #15118 ) ;
#5316 = ADVANCED_FACE ( 'NONE', ( #10447 ), #12520, .F. ) ;
#5317 = CARTESIAN_POINT ( 'NONE',  ( -18.86735971344653962, -5.080035572537331845, 56.85231026484398598 ) ) ;
#5318 = CARTESIAN_POINT ( 'NONE',  ( -22.58324314276470091, -9.630648466248954875, 56.85231026484398598 ) ) ;
#5319 = LINE ( 'NONE', #14802, #5324 ) ;
#5320 = CIRCLE ( 'NONE', #1418, 3.000000000000002665 ) ;
#5321 = EDGE_CURVE ( 'NONE', #13197, #6348, #6687, .T. ) ;
#5322 = FACE_OUTER_BOUND ( 'NONE', #9581, .T. ) ;
#5323 = CARTESIAN_POINT ( 'NONE',  ( 2.500300139188999182, -46.50737899243799944, 44.50231026484399877 ) ) ;
#5324 = VECTOR ( 'NONE', #4325, 1000.000000000000000 ) ;
#5325 = VERTEX_POINT ( 'NONE', #4641 ) ;
#5326 = DIRECTION ( 'NONE',  ( 0.000000000000000000, -1.000000000000000000, -1.224646799147350002E-16 ) ) ;
#5327 = CARTESIAN_POINT ( 'NONE',  ( -15.49969986081091378, -13.50737899243822859, 51.00031026484398922 ) ) ;
#5328 = ORIENTED_EDGE ( 'NONE', *, *, #10090, .F. ) ;
#5329 = CARTESIAN_POINT ( 'NONE',  ( -12.95343247850694723, -15.40470757524832912, 57.00231026484399166 ) ) ;
#5330 = LINE ( 'NONE', #4416, #5074 ) ;
#5331 = CARTESIAN_POINT ( 'NONE',  ( -27.49969986081100259, -57.00737899243800655, 55.03046811182510112 ) ) ;
#5332 = EDGE_LOOP ( 'NONE', ( #11663, #12308, #6014, #8597 ) ) ;
#5333 = PLANE ( 'NONE',  #6614 ) ;
#5334 = EDGE_CURVE ( 'NONE', #9659, #6512, #14635, .T. ) ;
#5335 = EDGE_CURVE ( 'NONE', #11647, #2093, #3473, .T. ) ;
#5336 = AXIS2_PLACEMENT_3D ( 'NONE', #11316, #3209, #13692 ) ;
#5337 = CARTESIAN_POINT ( 'NONE',  ( -24.06473463808513813, -13.92741382918746496, 56.85231026484398598 ) ) ;
#5338 = DIRECTION ( 'NONE',  ( 0.000000000000000000, 0.000000000000000000, -1.000000000000000000 ) ) ;
#5339 = CIRCLE ( 'NONE', #1668, 6.000000000000001776 ) ;
#5340 = FACE_OUTER_BOUND ( 'NONE', #3761, .T. ) ;
#5341 = PLANE ( 'NONE',  #12325 ) ;
#5342 = VERTEX_POINT ( 'NONE', #9680 ) ;
#5343 = CARTESIAN_POINT ( 'NONE',  ( -18.18846581869434686, -17.11577719991577951, 46.00231026484398456 ) ) ;
#5344 = CARTESIAN_POINT ( 'NONE',  ( -7.519587752637010070, -45.08058686818623784, -3.441745684778983794 ) ) ;
#5345 = ORIENTED_EDGE ( 'NONE', *, *, #4492, .F. ) ;
#5347 = ORIENTED_EDGE ( 'NONE', *, *, #13842, .T. ) ;
#5346 = DIRECTION ( 'NONE',  ( -1.734723475976807094E-16, 0.000000000000000000, 1.000000000000000000 ) ) ;
#5348 = ORIENTED_EDGE ( 'NONE', *, *, #12702, .F. ) ;
#5349 = CARTESIAN_POINT ( 'NONE',  ( -6.468284635389317749, -17.74225372801457112, 54.00231026484400587 ) ) ;
#5350 = DIRECTION ( 'NONE',  ( -1.000000000000000000, 0.000000000000000000, 0.000000000000000000 ) ) ;
#5351 = EDGE_CURVE ( 'NONE', #1855, #9677, #2346, .T. ) ;
#5352 = VECTOR ( 'NONE', #7271, 1000.000000000000114 ) ;
#5353 = DIRECTION ( 'NONE',  ( -8.018662683283438208E-16, 5.975035461963189015E-16, 1.000000000000000000 ) ) ;
#5354 = DIRECTION ( 'NONE',  ( 0.000000000000000000, 1.000000000000000000, 1.224646799147350002E-16 ) ) ;
#5355 = CARTESIAN_POINT ( 'NONE',  ( -13.18491133144367744, -15.23222315862922471, 56.75231026484399166 ) ) ;
#5356 = FACE_OUTER_BOUND ( 'NONE', #10252, .T. ) ;
#5357 = CONICAL_SURFACE ( 'NONE', #726, 8.314203600725839749, 0.8578293273552097808 ) ;
#5358 = DIRECTION ( 'NONE',  ( -0.5691548339926102429, -0.8222303661035904598, 3.489949670250058899E-17 ) ) ;
#5359 = VECTOR ( 'NONE', #11673, 1000.000000000000000 ) ;
#5360 = EDGE_CURVE ( 'NONE', #2549, #11181, #8452, .T. ) ;
#5361 = CARTESIAN_POINT ( 'NONE',  ( -15.49969986081099904, 20.99262100756200056, 24.21206422150099868 ) ) ;
#5362 = ORIENTED_EDGE ( 'NONE', *, *, #5321, .F. ) ;
#5363 = CARTESIAN_POINT ( 'NONE',  ( 14.95717157845075818, -28.53344780807426773, 46.08993571701573444 ) ) ;
#5364 = EDGE_LOOP ( 'NONE', ( #2458, #1604, #3129, #10667 ) ) ;
#5365 = DIRECTION ( 'NONE',  ( 1.000000000000000000, 1.201369187114119994E-15, 9.616040805000176517E-16 ) ) ;
#5367 = VERTEX_POINT ( 'NONE', #131 ) ;
#5366 = CARTESIAN_POINT ( 'NONE',  ( -7.532278898138853762, -45.22326128447397764, -7.645014517789088693 ) ) ;
#5368 = ORIENTED_EDGE ( 'NONE', *, *, #3536, .F. ) ;
#5369 = PLANE ( 'NONE',  #5557 ) ;
#5371 = ORIENTED_EDGE ( 'NONE', *, *, #8966, .T. ) ;
#5370 = CARTESIAN_POINT ( 'NONE',  ( -13.88982576282654691, -4.575998618238553917, 56.85231026484398598 ) ) ;
#5372 = FACE_OUTER_BOUND ( 'NONE', #7952, .T. ) ;
#5373 = FACE_OUTER_BOUND ( 'NONE', #13216, .T. ) ;
#5374 = CYLINDRICAL_SURFACE ( 'NONE', #13414, 0.2499999999999996947 ) ;
#5375 = AXIS2_PLACEMENT_3D ( 'NONE', #9514, #14184, #13125 ) ;
#5376 = CARTESIAN_POINT ( 'NONE',  ( 2.500300139188999182, -46.50737899243799944, 19.50231026484399877 ) ) ;
#5377 = EDGE_CURVE ( 'NONE', #11014, #8446, #9449, .T. ) ;
#5378 = PLANE ( 'NONE',  #12989 ) ;
#5379 = ORIENTED_EDGE ( 'NONE', *, *, #13881, .T. ) ;
#5380 = FACE_OUTER_BOUND ( 'NONE', #3100, .T. ) ;
#5381 = ORIENTED_EDGE ( 'NONE', *, *, #15020, .F. ) ;
#5382 = VERTEX_POINT ( 'NONE', #11823 ) ;
#5383 = PLANE ( 'NONE',  #14948 ) ;
#5384 = ORIENTED_EDGE ( 'NONE', *, *, #15059, .T. ) ;
#5385 = FACE_OUTER_BOUND ( 'NONE', #4754, .T. ) ;
#5386 = CIRCLE ( 'NONE', #13223, 6.828234652215419587 ) ;
#5387 = DIRECTION ( 'NONE',  ( 8.018662683283438208E-16, -5.975035461963189015E-16, -1.000000000000000000 ) ) ;
#5388 = DIRECTION ( 'NONE',  ( -8.018662683283439195E-16, 5.975035461963190001E-16, 1.000000000000000000 ) ) ;
#5389 = LINE ( 'NONE', #11213, #686 ) ;
#5390 = DIRECTION ( 'NONE',  ( 0.000000000000000000, 0.1872998510044495413, 0.9823027872370673208 ) ) ;
#5391 = EDGE_CURVE ( 'NONE', #8928, #572, #3716, .T. ) ;
#5393 = DIRECTION ( 'NONE',  ( 0.000000000000000000, 0.000000000000000000, -1.000000000000000000 ) ) ;
#5392 = CARTESIAN_POINT ( 'NONE',  ( -12.58343141761905670, -12.25091104594033098, 57.00231026484397745 ) ) ;
#5394 = ORIENTED_EDGE ( 'NONE', *, *, #10848, .T. ) ;
#5395 = FACE_OUTER_BOUND ( 'NONE', #7602, .T. ) ;
#5396 = DIRECTION ( 'NONE',  ( -0.9997391571607663341, -0.02283895005206026604, -7.880107536067206944E-16 ) ) ;
#5397 = ORIENTED_EDGE ( 'NONE', *, *, #227, .T. ) ;
#5398 = CARTESIAN_POINT ( 'NONE',  ( -10.72806301968316411, -20.63252684047564500, 56.85231026484400019 ) ) ;
#5399 = EDGE_CURVE ( 'NONE', #13689, #13829, #11054, .T. ) ;
#5400 = DIRECTION ( 'NONE',  ( -8.673617379884027583E-16, 1.000000000000000000, 0.000000000000000000 ) ) ;
#5401 = CARTESIAN_POINT ( 'NONE',  ( -5.526612771747951847, -13.70272205979775393, 54.00231026484399166 ) ) ;
#5402 = ORIENTED_EDGE ( 'NONE', *, *, #3652, .T. ) ;
#5403 = CARTESIAN_POINT ( 'NONE',  ( -17.40065610530428586, -5.145404622917534532, 56.85231026484398598 ) ) ;
#5404 = VECTOR ( 'NONE', #8068, 1000.000000000000000 ) ;
#5405 = DIRECTION ( 'NONE',  ( 1.000000000000000000, -1.291538348938060198E-32, 1.054621095516909827E-16 ) ) ;
#5406 = CARTESIAN_POINT ( 'NONE',  ( 0.8003001391889992266, 11.99262100756199878, 32.26206422150099939 ) ) ;
#5407 = CARTESIAN_POINT ( 'NONE',  ( 22.00030013918900096, -27.00737899243800300, 24.21206422150099868 ) ) ;
#5408 = EDGE_CURVE ( 'NONE', #6205, #9738, #14276, .T. ) ;
#5409 = DIRECTION ( 'NONE',  ( 0.7276687409742212953, 0.6859287159822015090, 1.736481776669299976E-16 ) ) ;
#5410 = VECTOR ( 'NONE', #8509, 1000.000000000000000 ) ;
#5411 = ORIENTED_EDGE ( 'NONE', *, *, #4857, .T. ) ;
#5412 = CARTESIAN_POINT ( 'NONE',  ( -28.28282149594069850, -32.00737899243799944, 54.75627176226269199 ) ) ;
#5413 = EDGE_CURVE ( 'NONE', #10807, #6204, #3564, .T. ) ;
#5414 = CARTESIAN_POINT ( 'NONE',  ( -15.61203582817000068, -107.1622034095870077, -6.087689735156000204 ) ) ;
#5415 = EDGE_CURVE ( 'NONE', #7352, #4490, #13138, .T. ) ;
#5416 = ORIENTED_EDGE ( 'NONE', *, *, #5133, .F. ) ;
#5418 = ORIENTED_EDGE ( 'NONE', *, *, #11972, .T. ) ;
#5417 = CARTESIAN_POINT ( 'NONE',  ( -7.512805849530849400, -44.04964101872660365, -5.039951761444699585 ) ) ;
#5419 = ORIENTED_EDGE ( 'NONE', *, *, #1134, .F. ) ;
#5420 = CARTESIAN_POINT ( 'NONE',  ( 9.000300139189000959, -27.00737899243800300, 43.21206422150100224 ) ) ;
#5421 = CARTESIAN_POINT ( 'NONE',  ( -14.44815700838962691, -52.45516431684754366, 56.99107276615496431 ) ) ;
#5422 = ADVANCED_FACE ( 'NONE', ( #11981, #51 ), #5022, .T. ) ;
#5423 = CIRCLE ( 'NONE', #3235, 3.000000000000002665 ) ;
#5424 = PLANE ( 'NONE',  #6393 ) ;
#5425 = CARTESIAN_POINT ( 'NONE',  ( -8.185742736628769833, -47.75198331066174262, 46.67630207578714163 ) ) ;
#5426 = VECTOR ( 'NONE', #2512, 1000.000000000000000 ) ;
#5427 = AXIS2_PLACEMENT_3D ( 'NONE', #4811, #2366, #8316 ) ;
#5428 = FACE_OUTER_BOUND ( 'NONE', #3936, .T. ) ;
#5429 = CYLINDRICAL_SURFACE ( 'NONE', #895, 8.000000000000000000 ) ;
#5430 = EDGE_CURVE ( 'NONE', #11463, #2715, #3868, .T. ) ;
#5431 = EDGE_CURVE ( 'NONE', #6794, #14079, #2488, .T. ) ;
#5432 = LINE ( 'NONE', #852, #7917 ) ;
#5433 = CARTESIAN_POINT ( 'NONE',  ( -15.83606446161809167, -16.37446674635458876, 56.89875687425071504 ) ) ;
#5434 = CARTESIAN_POINT ( 'NONE',  ( -14.10579935493720782, -22.47500361547664127, 57.00231026484399166 ) ) ;
#5435 = ORIENTED_EDGE ( 'NONE', *, *, #12415, .F. ) ;
#5436 = ORIENTED_EDGE ( 'NONE', *, *, #303, .T. ) ;
#5437 = ORIENTED_EDGE ( 'NONE', *, *, #4092, .F. ) ;
#5438 = VECTOR ( 'NONE', #13186, 1000.000000000000000 ) ;
#5439 = CARTESIAN_POINT ( 'NONE',  ( -7.838472470387507940, -46.81608433807591751, 17.01681591762138979 ) ) ;
#5441 = ORIENTED_EDGE ( 'NONE', *, *, #334, .T. ) ;
#5440 = CYLINDRICAL_SURFACE ( 'NONE', #10607, 10.00000000000000000 ) ;
#5442 = CARTESIAN_POINT ( 'NONE',  ( 9.000300139189000959, -19.50737899243800300, 24.21206422150099868 ) ) ;
#5443 = CARTESIAN_POINT ( 'NONE',  ( -9.969334273478565933, -7.622966832294271633, 57.00231026484397745 ) ) ;
#5444 = PRODUCT_RELATED_PRODUCT_CATEGORY ( 'part', '', ( #10297 ) ) ;
#5445 = EDGE_CURVE ( 'NONE', #12587, #9659, #2579, .T. ) ;
#5446 = CARTESIAN_POINT ( 'NONE',  ( -15.49969986081091378, -13.50737899243822859, 51.00031026484398922 ) ) ;
#5447 = AXIS2_PLACEMENT_3D ( 'NONE', #8328, #10709, #1224 ) ;
#5448 = VECTOR ( 'NONE', #7308, 1000.000000000000114 ) ;
#5449 = DIRECTION ( 'NONE',  ( -0.7511640317997414495, -0.6601155939154573771, -2.079116908177570050E-16 ) ) ;
#5450 = PLANE ( 'NONE',  #13508 ) ;
#5451 = VERTEX_POINT ( 'NONE', #7525 ) ;
#5452 = DIRECTION ( 'NONE',  ( 0.000000000000000000, 0.000000000000000000, 1.000000000000000000 ) ) ;
#5453 = VERTEX_POINT ( 'NONE', #1572 ) ;
#5454 = DIRECTION ( 'NONE',  ( 1.000000000000000000, -1.291538348938060198E-32, 1.054621095516909827E-16 ) ) ;
#5455 = EDGE_LOOP ( 'NONE', ( #8237, #6647, #13760, #9122 ) ) ;
#5456 = EDGE_LOOP ( 'NONE', ( #10483, #5094, #2062, #7611, #297 ) ) ;
#5457 = DIRECTION ( 'NONE',  ( 0.000000000000000000, 1.224646799147350002E-16, -1.000000000000000000 ) ) ;
#5458 = DIRECTION ( 'NONE',  ( -0.6601155939154559338, 0.7511640317997426708, -9.781476007338054812E-16 ) ) ;
#5459 = ORIENTED_EDGE ( 'NONE', *, *, #8796, .F. ) ;
#5460 = FACE_OUTER_BOUND ( 'NONE', #14290, .T. ) ;
#5461 = AXIS2_PLACEMENT_3D ( 'NONE', #6169, #223, #8240 ) ;
#5462 = EDGE_CURVE ( 'NONE', #13117, #14849, #10804, .T. ) ;
#5463 = FACE_OUTER_BOUND ( 'NONE', #5157, .T. ) ;
#5464 = LINE ( 'NONE', #15025, #6826 ) ;
#5465 = CIRCLE ( 'NONE', #596, 9.974999999999999645 ) ;
#5466 = CARTESIAN_POINT ( 'NONE',  ( -15.49969986081099904, 70.81438635534659909, 17.96206422150100579 ) ) ;
#5467 = AXIS2_PLACEMENT_3D ( 'NONE', #13968, #2348, #11670 ) ;
#5468 = DIRECTION ( 'NONE',  ( 8.018662683283438208E-16, -5.975035461963189015E-16, -1.000000000000000000 ) ) ;
#5470 = CARTESIAN_POINT ( 'NONE',  ( 4.965850942597395346, 5.948560758908072010, 29.50331482898986835 ) ) ;
#5469 = DIRECTION ( 'NONE',  ( 8.018662683283438208E-16, -5.975035461963189015E-16, -1.000000000000000000 ) ) ;
#5471 = EDGE_LOOP ( 'NONE', ( #932, #7215, #928, #2379 ) ) ;
#5472 = DIRECTION ( 'NONE',  ( 0.7032868978765922652, 0.7109061395677488404, 1.391731009600549485E-16 ) ) ;
#5473 = FACE_OUTER_BOUND ( 'NONE', #2414, .T. ) ;
#5474 = VERTEX_POINT ( 'NONE', #10904 ) ;
#5475 = ORIENTED_EDGE ( 'NONE', *, *, #1882, .F. ) ;
#5476 = CARTESIAN_POINT ( 'NONE',  ( 1.760741030006599317, 10.68321993080349763, 32.15417856559049881 ) ) ;
#5477 = LINE ( 'NONE', #1045, #7128 ) ;
#5478 = CARTESIAN_POINT ( 'NONE',  ( -7.886584594865190034, -46.96511696614940234, 17.04457229113261718 ) ) ;
#5479 = CARTESIAN_POINT ( 'NONE',  ( -15.61203582817000068, -106.2173407584721616, -5.758565883178085265 ) ) ;
#5480 = VECTOR ( 'NONE', #1844, 1000.000000000000114 ) ;
#5481 = ORIENTED_EDGE ( 'NONE', *, *, #11496, .T. ) ;
#5482 = DIRECTION ( 'NONE',  ( 0.8018662683283437342, -0.5975035461963190686, 1.000000000000000078E-15 ) ) ;
#5483 = VECTOR ( 'NONE', #3512, 1000.000000000000000 ) ;
#5484 = ADVANCED_FACE ( 'NONE', ( #7450 ), #432, .F. ) ;
#5485 = LINE ( 'NONE', #4345, #5129 ) ;
#5486 = CARTESIAN_POINT ( 'NONE',  ( 13.85920135429429934, -27.00737899243800300, 45.71206422150100224 ) ) ;
#5487 =( BOUNDED_CURVE ( )  B_SPLINE_CURVE ( 3, ( #6458, #1657, #1813, #10990 ),
 .UNSPECIFIED., .F., .T. ) 
 B_SPLINE_CURVE_WITH_KNOTS ( ( 4, 4 ),
 ( 5.074465175390796112, 5.274925224928544765 ),
 .UNSPECIFIED. ) 
 CURVE ( )  GEOMETRIC_REPRESENTATION_ITEM ( )  RATIONAL_B_SPLINE_CURVE ( ( 1.000000000000000000, 0.9966541165307394312, 0.9966541165307394312, 1.000000000000000000 ) ) 
 REPRESENTATION_ITEM ( '' )  );
#5488 = CARTESIAN_POINT ( 'NONE',  ( -14.61203582817000068, -107.9196643519486827, -5.433976602192393202 ) ) ;
#5489 = DIRECTION ( 'NONE',  ( 0.000000000000000000, 0.05233595624294329340, 0.9986295347545738332 ) ) ;
#5490 = EDGE_LOOP ( 'NONE', ( #11349, #13780, #10097, #12093 ) ) ;
#5491 = LINE ( 'NONE', #7479, #14360 ) ;
#5492 = CARTESIAN_POINT ( 'NONE',  ( -7.504307622470381745, -44.76319932751670194, -3.703265526006389141 ) ) ;
#5493 = AXIS2_PLACEMENT_3D ( 'NONE', #11763, #9470, #6092 ) ;
#5494 = ORIENTED_EDGE ( 'NONE', *, *, #9875, .F. ) ;
#5496 = VERTEX_POINT ( 'NONE', #11050 ) ;
#5495 = CARTESIAN_POINT ( 'NONE',  ( -15.49969986081099904, -26.50737899243800300, 19.50231026484400232 ) ) ;
#5497 = ORIENTED_EDGE ( 'NONE', *, *, #14487, .F. ) ;
#5498 = LINE ( 'NONE', #4433, #3969 ) ;
#5499 = CARTESIAN_POINT ( 'NONE',  ( -8.561607448813433052, -9.375294326971793879, 57.00231026484399166 ) ) ;
#5500 = EDGE_CURVE ( 'NONE', #1107, #1827, #11279, .T. ) ;
#5501 = CARTESIAN_POINT ( 'NONE',  ( -24.38380099443793725, -15.36048369738253427, 56.85231026484398598 ) ) ;
#5502 = CARTESIAN_POINT ( 'NONE',  ( -19.38713143869018296, -6.429305403720261936, 56.85231026484398598 ) ) ;
#5503 = EDGE_CURVE ( 'NONE', #8578, #12931, #2719, .T. ) ;
#5504 = CARTESIAN_POINT ( 'NONE',  ( -5.502541905842194936, -13.18104144132555078, 60.35493120382419363 ) ) ;
#5505 = CARTESIAN_POINT ( 'NONE',  ( -8.972439834930606040, -10.77678811232731348, 56.85231026484400019 ) ) ;
#5506 = CARTESIAN_POINT ( 'NONE',  ( -20.94048570341206883, -6.243833066724571168, 56.85231026484398598 ) ) ;
#5507 = EDGE_CURVE ( 'NONE', #11542, #364, #5310, .T. ) ;
#5508 = FACE_OUTER_BOUND ( 'NONE', #968, .T. ) ;
#5509 = CARTESIAN_POINT ( 'NONE',  ( 17.94012796689997558, -29.55659949177507073, 41.18440502598058828 ) ) ;
#5510 = LINE ( 'NONE', #2078, #2374 ) ;
#5512 = ORIENTED_EDGE ( 'NONE', *, *, #8138, .T. ) ;
#5511 = DIRECTION ( 'NONE',  ( 8.018662683283438208E-16, -5.975035461963189015E-16, -1.000000000000000000 ) ) ;
#5513 = ORIENTED_EDGE ( 'NONE', *, *, #7452, .T. ) ;
#5514 = DIRECTION ( 'NONE',  ( 0.5975035461963189576, 0.8018662683283437342, 0.000000000000000000 ) ) ;
#5515 = ORIENTED_EDGE ( 'NONE', *, *, #13342, .F. ) ;
#5516 = AXIS2_PLACEMENT_3D ( 'NONE', #7151, #3654, #10609 ) ;
#5517 = FACE_OUTER_BOUND ( 'NONE', #8032, .T. ) ;
#5518 = ADVANCED_FACE ( 'NONE', ( #647, #9971 ), #5383, .F. ) ;
#5519 = EDGE_CURVE ( 'NONE', #7300, #4677, #4692, .T. ) ;
#5520 = LINE ( 'NONE', #15081, #4774 ) ;
#5521 = CARTESIAN_POINT ( 'NONE',  ( -9.299228256956212135, -8.333850033420862502, 56.85231026484398598 ) ) ;
#5522 = VERTEX_POINT ( 'NONE', #4088 ) ;
#5523 = LINE ( 'NONE', #10033, #7356 ) ;
#5524 = CARTESIAN_POINT ( 'NONE',  ( -15.61203582817000068, -106.2504778273845147, -6.614114137688407169 ) ) ;
#5525 = EDGE_LOOP ( 'NONE', ( #1001, #13283, #7508, #7652, #6573 ) ) ;
#5526 = CARTESIAN_POINT ( 'NONE',  ( 15.30804704745935219, -24.78610190351696119, 45.59350641046059849 ) ) ;
#5527 = VERTEX_POINT ( 'NONE', #8747 ) ;
#5528 = LINE ( 'NONE', #9044, #3833 ) ;
#5529 = EDGE_LOOP ( 'NONE', ( #11024, #13365, #10902, #10652 ) ) ;
#5530 = VERTEX_POINT ( 'NONE', #14646 ) ;
#5531 = DIRECTION ( 'NONE',  ( -0.7737441449604661736, -0.6334982226805353500, -2.419218955996689845E-16 ) ) ;
#5532 = ORIENTED_EDGE ( 'NONE', *, *, #3966, .T. ) ;
#5533 = CARTESIAN_POINT ( 'NONE',  ( -9.658903420740534429, -39.03434883555972590, 56.54512877198791898 ) ) ;
#5534 = CIRCLE ( 'NONE', #6745, 6.250000000000001776 ) ;
#5535 =( NAMED_UNIT ( * ) SI_UNIT ( $, .STERADIAN. ) SOLID_ANGLE_UNIT ( ) );
#5536 = DIRECTION ( 'NONE',  ( 0.000000000000000000, -9.130123557772668334E-17, 1.000000000000000000 ) ) ;
#5537 = AXIS2_PLACEMENT_3D ( 'NONE', #11498, #7891, #12582 ) ;
#5538 = CARTESIAN_POINT ( 'NONE',  ( -23.36093307149983289, -11.66014798166512634, 56.85231026484398598 ) ) ;
#5539 = LINE ( 'NONE', #13734, #2784 ) ;
#5541 = LINE ( 'NONE', #10363, #8500 ) ;
#5540 = CARTESIAN_POINT ( 'NONE',  ( -23.39388780995641781, -11.80648316271623877, 57.00231026484397745 ) ) ;
#5542 = ORIENTED_EDGE ( 'NONE', *, *, #3646, .F. ) ;
#5543 = CARTESIAN_POINT ( 'NONE',  ( -7.529819136880052888, -45.22287388988081602, 42.34868737210720724 ) ) ;
#5544 = CIRCLE ( 'NONE', #7499, 8.000000000000000000 ) ;
#5545 = FACE_OUTER_BOUND ( 'NONE', #1847, .T. ) ;
#5546 = EDGE_LOOP ( 'NONE', ( #6723, #5877, #4678, #5962 ) ) ;
#5547 = ORIENTED_EDGE ( 'NONE', *, *, #3271, .T. ) ;
#5548 = CARTESIAN_POINT ( 'NONE',  ( -14.61203582816999891, -107.1622375242508696, -7.140479451889715889 ) ) ;
#5549 = EDGE_CURVE ( 'NONE', #5733, #8391, #13503, .T. ) ;
#5550 = EDGE_LOOP ( 'NONE', ( #12696, #15075 ) ) ;
#5551 = FACE_OUTER_BOUND ( 'NONE', #10237, .T. ) ;
#5552 = CARTESIAN_POINT ( 'NONE',  ( -6.368730986314239395, -9.491655842995189829, 57.00231026484399166 ) ) ;
#5553 = VECTOR ( 'NONE', #11238, 1000.000000000000227 ) ;
#5554 = CIRCLE ( 'NONE', #6767, 15.62500000000000000 ) ;
#5555 = PRODUCT_CONTEXT ( 'NONE', #1164, 'mechanical' ) ;
#5556 = DIRECTION ( 'NONE',  ( -0.1617534816134024167, 0.9868311969055004740, -7.193398003386505973E-16 ) ) ;
#5557 = AXIS2_PLACEMENT_3D ( 'NONE', #13708, #15003, #935 ) ;
#5558 = FACE_OUTER_BOUND ( 'NONE', #10411, .T. ) ;
#5559 = CARTESIAN_POINT ( 'NONE',  ( -23.05384319539488658, -10.65421522557165623, 56.85231026484398598 ) ) ;
#5560 = EDGE_LOOP ( 'NONE', ( #13557, #3905, #6494, #2824 ) ) ;
#5561 = CARTESIAN_POINT ( 'NONE',  ( -11.66301194181331979, -90.91152723309099315, -1.736239442649727627 ) ) ;
#5562 = CARTESIAN_POINT ( 'NONE',  ( -7.512025533959445056, -44.96883993545320379, -3.526982330024790446 ) ) ;
#5563 = LINE ( 'NONE', #10236, #13064 ) ;
#5564 = EDGE_CURVE ( 'NONE', #9069, #11272, #12058, .T. ) ;
#5565 = ORIENTED_EDGE ( 'NONE', *, *, #14451, .T. ) ;
#5566 = AXIS2_PLACEMENT_3D ( 'NONE', #13624, #2074, #771 ) ;
#5567 = ORIENTED_EDGE ( 'NONE', *, *, #662, .F. ) ;
#5568 = DIRECTION ( 'NONE',  ( 0.5975035461963189576, 0.8018662683283437342, 0.000000000000000000 ) ) ;
#5569 = CARTESIAN_POINT ( 'NONE',  ( -7.922155832732967973, -47.08606123773714813, 56.22882524374293212 ) ) ;
#5570 = CYLINDRICAL_SURFACE ( 'NONE', #2013, 19.00000000000000000 ) ;
#5571 = CARTESIAN_POINT ( 'NONE',  ( -8.551496829098008234, -48.47395512894357950, 42.95037523886164621 ) ) ;
#5572 =( BOUNDED_CURVE ( )  B_SPLINE_CURVE ( 3, ( #15113, #10604, #12911, #2423 ),
 .UNSPECIFIED., .F., .T. ) 
 B_SPLINE_CURVE_WITH_KNOTS ( ( 4, 4 ),
 ( 1.570796326794895670, 3.141592653589792228 ),
 .UNSPECIFIED. ) 
 CURVE ( )  GEOMETRIC_REPRESENTATION_ITEM ( )  RATIONAL_B_SPLINE_CURVE ( ( 1.000000000000000000, 0.8047378541243649375, 0.8047378541243649375, 1.000000000000000000 ) ) 
 REPRESENTATION_ITEM ( '' )  );
#5573 = VECTOR ( 'NONE', #10893, 1000.000000000000000 ) ;
#5574 = CARTESIAN_POINT ( 'NONE',  ( -7.977563667684565374, -6.908081013795536407, 60.95049943312243812 ) ) ;
#5575 = CIRCLE ( 'NONE', #5216, 1.750000000000000666 ) ;
#5576 = DIRECTION ( 'NONE',  ( 1.000000000000000000, 1.201369187114119994E-15, 9.616040805000176517E-16 ) ) ;
#5577 = CARTESIAN_POINT ( 'NONE',  ( -25.44713467170207366, -12.76632185356751847, 57.00231026484397745 ) ) ;
#5578 = DIRECTION ( 'NONE',  ( -0.9885168150181794511, 0.1511109077013120805, -8.829475928589259133E-16 ) ) ;
#5579 = EDGE_CURVE ( 'NONE', #1981, #7737, #14700, .T. ) ;
#5580 = ORIENTED_EDGE ( 'NONE', *, *, #12456, .F. ) ;
#5581 = CARTESIAN_POINT ( 'NONE',  ( 18.10161036139083990, -29.26328343019616085, 40.86242124114806273 ) ) ;
#5582 = AXIS2_PLACEMENT_3D ( 'NONE', #3579, #4962, #7159 ) ;
#5583 = ORIENTED_EDGE ( 'NONE', *, *, #1860, .T. ) ;
#5585 = ORIENTED_EDGE ( 'NONE', *, *, #8034, .F. ) ;
#5584 = DIRECTION ( 'NONE',  ( -8.018662683283438208E-16, 5.975035461963189015E-16, 1.000000000000000000 ) ) ;
#5586 = VERTEX_POINT ( 'NONE', #11204 ) ;
#5587 =( GEOMETRIC_REPRESENTATION_CONTEXT ( 3 ) GLOBAL_UNCERTAINTY_ASSIGNED_CONTEXT ( ( #7099 ) ) GLOBAL_UNIT_ASSIGNED_CONTEXT ( ( #3610, #6115, #12877 ) ) REPRESENTATION_CONTEXT ( 'NONE', 'WORKASPACE' ) );
#5588 = EDGE_CURVE ( 'NONE', #13722, #8988, #6133, .T. ) ;
#5589 = LINE ( 'NONE', #859, #12166 ) ;
#5590 = EDGE_LOOP ( 'NONE', ( #3961, #3752, #12160, #4795 ) ) ;
#5591 = B_SPLINE_CURVE_WITH_KNOTS ( 'NONE', 3,
 ( #8219, #2569, #4942, #3715, #11740, #7298, #12907, #9525, #3563, #2419, #1346, #11897, #6143, #1423, #1262, #5920, #4793, #14350, #6070, #10599, #10754, #3864, #278, #14120, #3640, #9602, #3792, #8451, #1945, #14570, #9756, #14423, #12280, #11129 ),
 .UNSPECIFIED., .F., .F.,
 ( 4, 2, 2, 2, 2, 2, 2, 2, 2, 2, 2, 2, 2, 2, 2, 2, 4 ),
 ( 0.000000000000000000, 0.0006405057738602453962, 0.001281011547720490792, 0.001921517321580736189, 0.002562023095440981585, 0.003202528869301226981, 0.003843034643161472377, 0.004483540417021717774, 0.005124046190881963170, 0.005764551964742208566, 0.006405057738602453962, 0.007045563512462699358, 0.007686069286322944755, 0.008326575060183191018, 0.008967080834043435547, 0.009607586607903680076, 0.01024809238176392634 ),
 .UNSPECIFIED. ) ;
#5592 = PLANE ( 'NONE',  #8771 ) ;
#5593 = B_SPLINE_CURVE_WITH_KNOTS ( 'NONE', 3,
 ( #2300, #11621, #5805, #2450, #163, #11855, #9, #9325, #10325, #8175, #12862, #2377, #9483, #7016, #11698, #1223, #13020, #14155, #14993, #5874, #3899, #14452, #3819, #13090, #7245, #2826, #12157, #10708, #1599, #14232, #9556, #9637, #2753, #12089, #7480, #11935 ),
 .UNSPECIFIED., .F., .F.,
 ( 4, 2, 1, 1, 1, 2, 2, 2, 1, 1, 1, 2, 2, 2, 2, 2, 2, 2, 2, 2, 4 ),
 ( 0.000000000000000000, 0.1249999999999846789, 0.1874999999999764910, 0.2187499999999724110, 0.2343749999999710232, 0.2421874999999706624, 0.2499999999999703015, 0.3749999999999719669, 0.4374999999999742983, 0.4687499999999745759, 0.4843749999999745204, 0.4921874999999732991, 0.4999999999999720224, 0.6249999999999749090, 0.6874999999999754641, 0.7187499999999766853, 0.7499999999999780176, 0.8124999999999826805, 0.8437499999999856781, 0.8749999999999887867, 1.000000000000000000 ),
 .UNSPECIFIED. ) ;
#5594 = DIRECTION ( 'NONE',  ( 1.000000000000000000, 1.000000000000000078E-15, 0.000000000000000000 ) ) ;
#5595 = VECTOR ( 'NONE', #2390, 1000.000000000000000 ) ;
#5596 = CIRCLE ( 'NONE', #8536, 3.000000000000002665 ) ;
#5597 = ORIENTED_EDGE ( 'NONE', *, *, #5351, .T. ) ;
#5598 = DIRECTION ( 'NONE',  ( 0.5975035461963189576, 0.8018662683283437342, 0.000000000000000000 ) ) ;
#5599 = EDGE_CURVE ( 'NONE', #4546, #6222, #15021, .T. ) ;
#5600 = EDGE_LOOP ( 'NONE', ( #13286, #12388 ) ) ;
#5601 = CARTESIAN_POINT ( 'NONE',  ( -2.716578225681299141, -32.00737899243799944, -17.99768973515599768 ) ) ;
#5602 = EDGE_CURVE ( 'NONE', #2901, #5814, #10276, .T. ) ;
#5603 = VERTEX_POINT ( 'NONE', #1946 ) ;
#5604 = CARTESIAN_POINT ( 'NONE',  ( -23.45327702811275827, -7.487309620431346069, 56.85231026484398598 ) ) ;
#5605 = ORIENTED_EDGE ( 'NONE', *, *, #10527, .F. ) ;
#5606 = ORIENTED_EDGE ( 'NONE', *, *, #4087, .F. ) ;
#5607 = CARTESIAN_POINT ( 'NONE',  ( 2.788504248039533451, -40.33206847769235992, 52.24055437141020519 ) ) ;
#5608 = ORIENTED_EDGE ( 'NONE', *, *, #13711, .F. ) ;
#5609 = VECTOR ( 'NONE', #6452, 1000.000000000000000 ) ;
#5610 = CYLINDRICAL_SURFACE ( 'NONE', #2272, 0.2000000000000012046 ) ;
#5611 = CARTESIAN_POINT ( 'NONE',  ( -15.49969986081099904, -13.50737899243800122, 54.00231026484400587 ) ) ;
#5612 = CARTESIAN_POINT ( 'NONE',  ( -10.35395692991667360, -90.56631534932571981, -7.082904691259424901 ) ) ;
#5613 = CARTESIAN_POINT ( 'NONE',  ( -7.660976687611689151, -46.08634367607207594, 21.96889143210171014 ) ) ;
#5615 = DIRECTION ( 'NONE',  ( 0.9320450512859429493, -0.1645000119736390598, 0.3228494516551898008 ) ) ;
#5614 = DIRECTION ( 'NONE',  ( -0.6251242923673536733, -0.7805252200231682647, -3.489949670250128540E-17 ) ) ;
#5616 = ORIENTED_EDGE ( 'NONE', *, *, #4898, .F. ) ;
#5617 = CARTESIAN_POINT ( 'NONE',  ( -23.96284084890188382, -10.23071992935364527, 56.85231026484398598 ) ) ;
#5618 = ADVANCED_FACE ( 'NONE', ( #12501, #7743 ), #4316, .T. ) ;
#5619 = ADVANCED_FACE ( 'NONE', ( #13875 ), #4545, .T. ) ;
#5620 = FACE_OUTER_BOUND ( 'NONE', #9900, .T. ) ;
#5621 = VERTEX_POINT ( 'NONE', #13802 ) ;
#5622 = ORIENTED_EDGE ( 'NONE', *, *, #1535, .T. ) ;
#5623 = CARTESIAN_POINT ( 'NONE',  ( -15.49969986081099904, -27.00737899243800300, -5.497689735156002122 ) ) ;
#5624 = EDGE_CURVE ( 'NONE', #11420, #6835, #4469, .T. ) ;
#5625 = AXIS2_PLACEMENT_3D ( 'NONE', #174, #5972, #2613 ) ;
#5626 = CARTESIAN_POINT ( 'NONE',  ( -20.37940433654428318, -38.14658552601336083, -17.68140352835245110 ) ) ;
#5627 = DIRECTION ( 'NONE',  ( 1.000000000000000000, -1.499759782661860071E-32, 1.224646799147350002E-16 ) ) ;
#5628 = VERTEX_POINT ( 'NONE', #7813 ) ;
#5629 = DIRECTION ( 'NONE',  ( 1.000000000000000000, 1.201369187114119994E-15, 9.616040805000176517E-16 ) ) ;
#5630 = LINE ( 'NONE', #2046, #14649 ) ;
#5631 = ITEM_DEFINED_TRANSFORMATION ( 'NONE', 'NONE', #8531,  #6789 ) ;
#5632 = EDGE_CURVE ( 'NONE', #14564, #8987, #6894, .T. ) ;
#5633 = CARTESIAN_POINT ( 'NONE',  ( -7.658052939403637183, -48.44202655475336172, 21.08574281859059241 ) ) ;
#5634 = DIRECTION ( 'NONE',  ( -1.000000000000000000, -3.632077277826439854E-16, 0.000000000000000000 ) ) ;
#5635 = CARTESIAN_POINT ( 'NONE',  ( -35.18530787408519700, 11.99262100756819827, 32.26206422150099939 ) ) ;
#5636 = ORIENTED_EDGE ( 'NONE', *, *, #14166, .F. ) ;
#5637 = CARTESIAN_POINT ( 'NONE',  ( -10.12676381431746542, -90.53940471697117687, -5.497640657892870486 ) ) ;
#5638 = CARTESIAN_POINT ( 'NONE',  ( -33.37394235882850069, 7.183219930803497633, 30.65500261342018007 ) ) ;
#5639 = CARTESIAN_POINT ( 'NONE',  ( 22.00030013918900096, -27.00737899243800300, 8.462064221501000461 ) ) ;
#5640 = CARTESIAN_POINT ( 'NONE',  ( -15.47724068538499154, -13.46270701644446177, 56.85231026484398598 ) ) ;
#5641 = EDGE_LOOP ( 'NONE', ( #678, #10792, #5842, #14157 ) ) ;
#5642 = CYLINDRICAL_SURFACE ( 'NONE', #4246, 2.499999999999998668 ) ;
#5643 = ORIENTED_EDGE ( 'NONE', *, *, #1162, .T. ) ;
#5644 = CIRCLE ( 'NONE', #9557, 0.4500000000000011768 ) ;
#5645 = LINE ( 'NONE', #10316, #3729 ) ;
#5646 = DIRECTION ( 'NONE',  ( 8.018662683283438208E-16, -5.975035461963189015E-16, -1.000000000000000000 ) ) ;
#5647 = CARTESIAN_POINT ( 'NONE',  ( -17.20133171717847631, -6.639650181150215325, 57.00231026484397745 ) ) ;
#5648 = CARTESIAN_POINT ( 'NONE',  ( -8.370866812342363517, -48.14008301383953636, 42.60233345630671664 ) ) ;
#5649 = EDGE_CURVE ( 'NONE', #14723, #11853, #4948, .T. ) ;
#5650 = DIRECTION ( 'NONE',  ( 0.000000000000000000, 0.000000000000000000, -1.000000000000000000 ) ) ;
#5651 = CIRCLE ( 'NONE', #6864, 1.599999999999999201 ) ;
#5652 = CARTESIAN_POINT ( 'NONE',  ( -9.401538680480957311, -6.786242167561306715, 56.85231026484398598 ) ) ;
#5653 = CARTESIAN_POINT ( 'NONE',  ( -31.79969986081099975, 3.992621007561997892, 24.26206422150100650 ) ) ;
#5654 = DIRECTION ( 'NONE',  ( -8.018662683283438208E-16, 5.975035461963189015E-16, 1.000000000000000000 ) ) ;
#5655 = ORIENTED_EDGE ( 'NONE', *, *, #13938, .T. ) ;
#5656 = CARTESIAN_POINT ( 'NONE',  ( 16.55417383883170857, -30.23012602008740757, 43.67615232897840372 ) ) ;
#5657 = ORIENTED_EDGE ( 'NONE', *, *, #13777, .T. ) ;
#5659 = ORIENTED_EDGE ( 'NONE', *, *, #7037, .F. ) ;
#5658 = CARTESIAN_POINT ( 'NONE',  ( -25.36033965610130991, -11.87119290823832252, 60.39242409889988750 ) ) ;
#5660 = ORIENTED_EDGE ( 'NONE', *, *, #14451, .F. ) ;
#5661 = DIRECTION ( 'NONE',  ( 0.9320450512859435044, -0.1973458207444490631, -0.3038859151196097730 ) ) ;
#5662 = AXIS2_PLACEMENT_3D ( 'NONE', #8047, #8970, #3167 ) ;
#5663 = FACE_OUTER_BOUND ( 'NONE', #7874, .T. ) ;
#5664 = VERTEX_POINT ( 'NONE', #6823 ) ;
#5665 =( BOUNDED_CURVE ( )  B_SPLINE_CURVE ( 3, ( #7852, #12548, #9088, #12623 ),
 .UNSPECIFIED., .F., .T. ) 
 B_SPLINE_CURVE_WITH_KNOTS ( ( 4, 4 ),
 ( 1.023945376098953863, 1.222940073837788688 ),
 .UNSPECIFIED. ) 
 CURVE ( )  GEOMETRIC_REPRESENTATION_ITEM ( )  RATIONAL_B_SPLINE_CURVE ( ( 1.000000000000000000, 0.9967028139718016044, 0.9967028139718016044, 1.000000000000000000 ) ) 
 REPRESENTATION_ITEM ( '' )  );
#5666 = VECTOR ( 'NONE', #451, 1000.000000000000114 ) ;
#5667 = PLANE ( 'NONE',  #13436 ) ;
#5668 = AXIS2_PLACEMENT_3D ( 'NONE', #3210, #7708, #1837 ) ;
#5669 = ADVANCED_FACE ( 'NONE', ( #14795 ), #12586, .F. ) ;
#5670 = DIRECTION ( 'NONE',  ( -8.673617379884027583E-16, 1.000000000000000000, 0.000000000000000000 ) ) ;
#5671 = ADVANCED_FACE ( 'NONE', ( #1097 ), #13730, .F. ) ;
#5672 = AXIS2_PLACEMENT_3D ( 'NONE', #1950, #4894, #6301 ) ;
#5673 = EDGE_LOOP ( 'NONE', ( #110, #10532, #5381, #12847, #12734 ) ) ;
#5674 = VECTOR ( 'NONE', #7644, 1000.000000000000000 ) ;
#5675 = DIRECTION ( 'NONE',  ( 0.000000000000000000, -1.000000000000000000, -1.224646799147350002E-16 ) ) ;
#5676 = ORIENTED_EDGE ( 'NONE', *, *, #7323, .F. ) ;
#5677 = LINE ( 'NONE', #15013, #12507 ) ;
#5678 = VERTEX_POINT ( 'NONE', #4242 ) ;
#5679 = DIRECTION ( 'NONE',  ( 8.018662683283438208E-16, -5.975035461963189015E-16, -1.000000000000000000 ) ) ;
#5680 = ORIENTED_EDGE ( 'NONE', *, *, #5742, .F. ) ;
#5681 = ORIENTED_EDGE ( 'NONE', *, *, #474, .F. ) ;
#5682 = CARTESIAN_POINT ( 'NONE',  ( -8.525484111995742964, -7.700351810740323266, 56.85231026484400019 ) ) ;
#5683 = ORIENTED_EDGE ( 'NONE', *, *, #1162, .F. ) ;
#5684 = LINE ( 'NONE', #10201, #13507 ) ;
#5685 = VECTOR ( 'NONE', #3824, 1000.000000000000000 ) ;
#5686 = ADVANCED_FACE ( 'NONE', ( #11354 ), #10352, .T. ) ;
#5687 = SURFACE_STYLE_USAGE ( .BOTH. , #10122 ) ;
#5688 = DIRECTION ( 'NONE',  ( 8.018662683283438208E-16, -5.975035461963189015E-16, -1.000000000000000000 ) ) ;
#5689 = ADVANCED_FACE ( 'NONE', ( #11275 ), #2021, .T. ) ;
#5690 = EDGE_CURVE ( 'NONE', #2418, #9903, #14607, .T. ) ;
#5691 = CARTESIAN_POINT ( 'NONE',  ( -7.640766570737479668, -45.98099911298281484, 21.94864471303565878 ) ) ;
#5693 = CARTESIAN_POINT ( 'NONE',  ( 2.374542637206501272, 7.183219930803497633, 30.65500261342018007 ) ) ;
#5692 = CARTESIAN_POINT ( 'NONE',  ( -21.23124220554638697, -20.54376104222092181, 57.00231026484397745 ) ) ;
#5694 = ORIENTED_EDGE ( 'NONE', *, *, #5168, .T. ) ;
#5695 = LINE ( 'NONE', #889, #12903 ) ;
#5696 = FACE_OUTER_BOUND ( 'NONE', #4122, .T. ) ;
#5697 = ORIENTED_EDGE ( 'NONE', *, *, #6289, .T. ) ;
#5698 = EDGE_CURVE ( 'NONE', #9250, #8623, #8435, .T. ) ;
#5699 = ORIENTED_EDGE ( 'NONE', *, *, #10032, .F. ) ;
#5700 = DIRECTION ( 'NONE',  ( -1.000000000000000000, -1.201369187114119994E-15, -9.616040805000176517E-16 ) ) ;
#5701 = CIRCLE ( 'NONE', #11090, 37.50000000000000711 ) ;
#5702 = VECTOR ( 'NONE', #4030, 1000.000000000000000 ) ;
#5703 = CARTESIAN_POINT ( 'NONE',  ( -22.43025610151164173, -40.50285774858512866, -17.35190600379631221 ) ) ;
#5704 = CARTESIAN_POINT ( 'NONE',  ( -15.49969986081099904, -2.007378992438005216, 61.71206422150100934 ) ) ;
#5705 = ORIENTED_EDGE ( 'NONE', *, *, #6357, .F. ) ;
#5706 = CARTESIAN_POINT ( 'NONE',  ( 7.500245791298697284, 3.992621007561997892, 24.16206422150099442 ) ) ;
#5707 = EDGE_CURVE ( 'NONE', #10582, #13608, #4926, .T. ) ;
#5708 = DIRECTION ( 'NONE',  ( -1.000000000000000000, -1.201369187114119994E-15, -9.616040805000176517E-16 ) ) ;
#5709 = ADVANCED_FACE ( 'NONE', ( #13044 ), #7123, .T. ) ;
#5710 = AXIS2_PLACEMENT_3D ( 'NONE', #4151, #11111, #13141 ) ;
#5711 = DIRECTION ( 'NONE',  ( 0.9931883319083343320, -0.1165201156931293391, 8.660254037844386422E-16 ) ) ;
#5712 = CARTESIAN_POINT ( 'NONE',  ( -7.499699860810997265, -44.50737899243797813, 46.00231026484399877 ) ) ;
#5713 = ORIENTED_EDGE ( 'NONE', *, *, #13693, .F. ) ;
#5714 = CARTESIAN_POINT ( 'NONE',  ( -11.75214016307909581, -90.94766999248710704, -1.647608471205698644 ) ) ;
#5715 = CARTESIAN_POINT ( 'NONE',  ( -5.499699860811000818, -46.50737899243799944, 22.00231026484399877 ) ) ;
#5716 = AXIS2_PLACEMENT_3D ( 'NONE', #13280, #12273, #5151 ) ;
#5717 = DIRECTION ( 'NONE',  ( 0.000000000000000000, 0.000000000000000000, -1.000000000000000000 ) ) ;
#5718 = DIRECTION ( 'NONE',  ( 0.5975035461963189576, 0.8018662683283437342, 0.000000000000000000 ) ) ;
#5719 = ORIENTED_EDGE ( 'NONE', *, *, #13379, .T. ) ;
#5720 = DIRECTION ( 'NONE',  ( -8.018662683283438208E-16, 5.975035461963189015E-16, 1.000000000000000000 ) ) ;
#5721 = ORIENTED_EDGE ( 'NONE', *, *, #117, .F. ) ;
#5722 = EDGE_CURVE ( 'NONE', #10422, #1909, #1171, .T. ) ;
#5723 = CIRCLE ( 'NONE', #3760, 28.00000000000000000 ) ;
#5724 = CARTESIAN_POINT ( 'NONE',  ( -7.512805849530849400, -44.04964101872660365, 19.96004823855532706 ) ) ;
#5725 = CARTESIAN_POINT ( 'NONE',  ( -5.499699860811000818, -46.50737899243799944, 19.50231026484399877 ) ) ;
#5726 = CARTESIAN_POINT ( 'NONE',  ( -23.09568838840838012, -16.24821979201191979, 56.85231026484398598 ) ) ;
#5727 = PLANE ( 'NONE',  #6215 ) ;
#5728 = DIRECTION ( 'NONE',  ( -8.018662683283438208E-16, 5.975035461963189015E-16, 1.000000000000000000 ) ) ;
#5729 = VECTOR ( 'NONE', #12247, 1000.000000000000000 ) ;
#5730 = DIRECTION ( 'NONE',  ( 9.999999999999998805E-16, -0.05233595624294299503, -0.9986295347545739443 ) ) ;
#5731 = CARTESIAN_POINT ( 'NONE',  ( -17.95685260396765770, -23.17500669507538191, 54.00231026484399166 ) ) ;
#5732 = DIRECTION ( 'NONE',  ( 0.000000000000000000, 1.369518533665900312E-16, -1.000000000000000000 ) ) ;
#5733 = VERTEX_POINT ( 'NONE', #13949 ) ;
#5734 = CARTESIAN_POINT ( 'NONE',  ( -8.600581100527527667, -9.311215824554304632, 56.85231026484400019 ) ) ;
#5735 = UNCERTAINTY_MEASURE_WITH_UNIT (LENGTH_MEASURE( 1.000000000000000082E-05 ), #10106, 'distance_accuracy_value', 'NONE');
#5736 = VERTEX_POINT ( 'NONE', #4619 ) ;
#5737 = LINE ( 'NONE', #13783, #11904 ) ;
#5739 = ORIENTED_EDGE ( 'NONE', *, *, #7835, .F. ) ;
#5738 = CARTESIAN_POINT ( 'NONE',  ( -25.43050946283875646, -12.36304378589120745, 60.37322180574037134 ) ) ;
#5740 = EDGE_CURVE ( 'NONE', #4983, #13470, #9277, .T. ) ;
#5741 = EDGE_LOOP ( 'NONE', ( #14458, #7918, #10873, #14995 ) ) ;
#5742 = EDGE_CURVE ( 'NONE', #13944, #2941, #13119, .T. ) ;
#5743 = CARTESIAN_POINT ( 'NONE',  ( -14.61203582817000068, -106.7406604375499626, -7.297873098422155813 ) ) ;
#5744 = ORIENTED_EDGE ( 'NONE', *, *, #8772, .F. ) ;
#5745 = DIRECTION ( 'NONE',  ( 0.000000000000000000, 1.850371707708594316E-16, -1.000000000000000000 ) ) ;
#5746 = CYLINDRICAL_SURFACE ( 'NONE', #12591, 6.000000000000000000 ) ;
#5747 = LINE ( 'NONE', #9264, #4662 ) ;
#5748 = CARTESIAN_POINT ( 'NONE',  ( -14.99866629829804765, -4.445910272123860807, 56.85231026484398598 ) ) ;
#5749 = ORIENTED_EDGE ( 'NONE', *, *, #14302, .F. ) ;
#5750 = DIRECTION ( 'NONE',  ( 0.5975035461963189576, 0.8018662683283437342, 0.000000000000000000 ) ) ;
#5751 = EDGE_LOOP ( 'NONE', ( #3794, #6333 ) ) ;
#5752 =( BOUNDED_CURVE ( )  B_SPLINE_CURVE ( 3, ( #12719, #10099, #3228, #14927 ),
 .UNSPECIFIED., .F., .T. ) 
 B_SPLINE_CURVE_WITH_KNOTS ( ( 4, 4 ),
 ( 5.266983419591705129, 7.299387194767472664 ),
 .UNSPECIFIED. ) 
 CURVE ( )  GEOMETRIC_REPRESENTATION_ITEM ( )  RATIONAL_B_SPLINE_CURVE ( ( 1.000000000000000000, 0.6843990470536898130, 0.6843990470536898130, 1.000000000000000000 ) ) 
 REPRESENTATION_ITEM ( '' )  );
#5753 = DIRECTION ( 'NONE',  ( 0.5975035461963189576, 0.8018662683283437342, 0.000000000000000000 ) ) ;
#5754 = ORIENTED_EDGE ( 'NONE', *, *, #2725, .F. ) ;
#5755 = ORIENTED_EDGE ( 'NONE', *, *, #9933, .F. ) ;
#5756 = ADVANCED_FACE ( 'NONE', ( #3468 ), #4853, .F. ) ;
#5757 = B_SPLINE_CURVE_WITH_KNOTS ( 'NONE', 3,
 ( #15067, #12790, #1140, #12944, #10631, #2524, #3440, #4669, #7175, #9248 ),
 .UNSPECIFIED., .F., .F.,
 ( 4, 2, 2, 2, 4 ),
 ( 0.000000000000000000, 0.0005837886004704026912, 0.001167577200940805382, 0.001751365801411208182, 0.002335154401881610765 ),
 .UNSPECIFIED. ) ;
#5758 = DIRECTION ( 'NONE',  ( 1.000000000000000000, 1.000000000000000078E-15, 1.000000000000000078E-15 ) ) ;
#5759 = ORIENTED_EDGE ( 'NONE', *, *, #12846, .T. ) ;
#5760 = CARTESIAN_POINT ( 'NONE',  ( -9.150909411738691546, -39.63286124672721655, 56.46135555955575569 ) ) ;
#5761 = CARTESIAN_POINT ( 'NONE',  ( -10.12827359990930987, -90.53873857836721584, -5.509565971075029545 ) ) ;
#5762 = CARTESIAN_POINT ( 'NONE',  ( -19.27841348868324545, -22.73895244004356897, 57.00231026484399166 ) ) ;
#5764 = DIRECTION ( 'NONE',  ( -1.000000000000000000, 0.000000000000000000, 0.000000000000000000 ) ) ;
#5763 = DIRECTION ( 'NONE',  ( -8.018662683283439195E-16, 5.975035461963190001E-16, 1.000000000000000000 ) ) ;
#5765 = ORIENTED_EDGE ( 'NONE', *, *, #13391, .T. ) ;
#5766 = CARTESIAN_POINT ( 'NONE',  ( -7.663084634444070176, -46.12710533971196014, 42.02396812144193916 ) ) ;
#5767 = DIRECTION ( 'NONE',  ( -8.018662683283438208E-16, 5.975035461963189015E-16, 1.000000000000000000 ) ) ;
#5768 = VERTEX_POINT ( 'NONE', #7277 ) ;
#5769 = ORIENTED_EDGE ( 'NONE', *, *, #8102, .F. ) ;
#5770 = CYLINDRICAL_SURFACE ( 'NONE', #5910, 8.000000000000000000 ) ;
#5771 = EDGE_CURVE ( 'NONE', #5474, #2398, #3776, .T. ) ;
#5772 = CARTESIAN_POINT ( 'NONE',  ( -23.24232539787402274, -42.42616270815122448, -17.18982661429730641 ) ) ;
#5773 = VECTOR ( 'NONE', #14917, 1000.000000000000000 ) ;
#5774 = ORIENTED_EDGE ( 'NONE', *, *, #6613, .F. ) ;
#5775 = LINE ( 'NONE', #10449, #4251 ) ;
#5776 = ORIENTED_EDGE ( 'NONE', *, *, #2574, .T. ) ;
#5777 = CARTESIAN_POINT ( 'NONE',  ( -17.81448839017816610, -11.78253482624722537, 51.00231026484399166 ) ) ;
#5778 = EDGE_CURVE ( 'NONE', #5017, #2405, #9507, .T. ) ;
#5779 = DIRECTION ( 'NONE',  ( 0.000000000000000000, 0.1872998510044759646, 0.9823027872370621028 ) ) ;
#5780 = CARTESIAN_POINT ( 'NONE',  ( -15.61203582817000246, -106.3249253597797406, -5.117531130952053253 ) ) ;
#5781 = VECTOR ( 'NONE', #235, 1000.000000000000000 ) ;
#5782 = CARTESIAN_POINT ( 'NONE',  ( -27.49969986081100259, -57.00737899243800655, -16.02584758213710003 ) ) ;
#5783 = ORIENTED_EDGE ( 'NONE', *, *, #14809, .T. ) ;
#5784 = CARTESIAN_POINT ( 'NONE',  ( -10.14594238360923129, -90.54069878331144139, -4.997746991299526265 ) ) ;
#5785 = CARTESIAN_POINT ( 'NONE',  ( -22.58324314276470091, -9.630648466248954875, 56.85231026484398598 ) ) ;
#5786 = DIRECTION ( 'NONE',  ( -0.6061090314442014737, 0.7953815700667020705, -9.612616959383187437E-16 ) ) ;
#5787 = VECTOR ( 'NONE', #1470, 1000.000000000000114 ) ;
#5788 = EDGE_CURVE ( 'NONE', #3714, #7506, #3698, .T. ) ;
#5790 = EDGE_CURVE ( 'NONE', #11735, #10731, #11881, .T. ) ;
#5789 = DIRECTION ( 'NONE',  ( 0.5104125104778984845, 0.8599296884906632021, -1.045284632676530333E-16 ) ) ;
#5791 = EDGE_LOOP ( 'NONE', ( #8798, #11859, #340, #12751, #1656, #6339, #5328 ) ) ;
#5792 = CARTESIAN_POINT ( 'NONE',  ( -7.499699860810997265, -44.50737899243797813, 46.00231026484399877 ) ) ;
#5793 = EDGE_LOOP ( 'NONE', ( #7386, #874, #1373, #6825, #3334 ) ) ;
#5794 = LINE ( 'NONE', #3508, #2256 ) ;
#5795 = DIRECTION ( 'NONE',  ( -1.000000000000000000, 0.000000000000000000, -9.688619527525975741E-16 ) ) ;
#5796 = CONICAL_SURFACE ( 'NONE', #9715, 0.9999999999999990008, 0.7853981633974476129 ) ;
#5797 = VECTOR ( 'NONE', #8154, 1000.000000000000000 ) ;
#5798 = CARTESIAN_POINT ( 'NONE',  ( -23.68291657637574588, -19.21137664199072148, 57.00231026484397745 ) ) ;
#5799 =( LENGTH_UNIT ( ) NAMED_UNIT ( * ) SI_UNIT ( .MILLI., .METRE. ) );
#5800 = CARTESIAN_POINT ( 'NONE',  ( -14.61203582817000068, -107.8822043817477976, -5.237516044744977783 ) ) ;
#5801 = CARTESIAN_POINT ( 'NONE',  ( -15.49969986081099904, 0.9926210075619958939, 47.21206422150099513 ) ) ;
#5802 = CARTESIAN_POINT ( 'NONE',  ( -13.57551609484869637, -3.719726473329906025, 54.00231026484399166 ) ) ;
#5803 = CIRCLE ( 'NONE', #13636, 0.4500000000000011768 ) ;
#5804 = CIRCLE ( 'NONE', #7262, 37.50000000000000000 ) ;
#5805 = CARTESIAN_POINT ( 'NONE',  ( -37.91145957496917163, -37.03279448458209799, 49.57038636259010644 ) ) ;
#5806 = FACE_OUTER_BOUND ( 'NONE', #1094, .T. ) ;
#5807 = VECTOR ( 'NONE', #11589, 1000.000000000000000 ) ;
#5808 = ORIENTED_EDGE ( 'NONE', *, *, #2915, .F. ) ;
#5809 = LINE ( 'NONE', #6537, #301 ) ;
#5810 = EDGE_CURVE ( 'NONE', #2175, #12515, #6330, .T. ) ;
#5811 = EDGE_LOOP ( 'NONE', ( #6441, #4693, #9842, #11479 ) ) ;
#5813 = ORIENTED_EDGE ( 'NONE', *, *, #10982, .F. ) ;
#5812 = CARTESIAN_POINT ( 'NONE',  ( -17.77108926314113191, -3.766888484081842403, 61.64460505631792842 ) ) ;
#5814 = VERTEX_POINT ( 'NONE', #14333 ) ;
#5815 = FACE_OUTER_BOUND ( 'NONE', #13045, .T. ) ;
#5816 = VERTEX_POINT ( 'NONE', #1853 ) ;
#5817 = CARTESIAN_POINT ( 'NONE',  ( -15.12053853660593283, -5.441285657357897598, 57.00231026484397745 ) ) ;
#5818 = DIRECTION ( 'NONE',  ( 0.8885476655824650072, 0.4587843131450243805, 4.383711467890778149E-16 ) ) ;
#5819 = CARTESIAN_POINT ( 'NONE',  ( -15.61203582817000068, -107.1621692949231459, -5.034900018422284518 ) ) ;
#5820 = CARTESIAN_POINT ( 'NONE',  ( 17.66455568904909512, -24.11403567254761171, 6.707112557092502314 ) ) ;
#5821 = EDGE_CURVE ( 'NONE', #13135, #6106, #9661, .T. ) ;
#5822 = DIRECTION ( 'NONE',  ( -0.3956847857120158740, 0.9183863840214728791, 0.000000000000000000 ) ) ;
#5823 = DIRECTION ( 'NONE',  ( -8.018662683283438208E-16, 5.975035461963189015E-16, 1.000000000000000000 ) ) ;
#5824 = ORIENTED_EDGE ( 'NONE', *, *, #2384, .T. ) ;
#5825 = CARTESIAN_POINT ( 'NONE',  ( -14.04983158491594075, -17.77761107388303685, -13.26088994341721694 ) ) ;
#5826 = ORIENTED_EDGE ( 'NONE', *, *, #2712, .T. ) ;
#5827 = DIRECTION ( 'NONE',  ( -1.000000000000000000, -3.700743415417187646E-16, 0.000000000000000000 ) ) ;
#5828 = VERTEX_POINT ( 'NONE', #9810 ) ;
#5829 = ORIENTED_EDGE ( 'NONE', *, *, #10184, .F. ) ;
#5830 = CARTESIAN_POINT ( 'NONE',  ( -20.48903913017556633, -19.85700446605285308, 56.85231026484398598 ) ) ;
#5831 = ORIENTED_EDGE ( 'NONE', *, *, #10247, .T. ) ;
#5832 = FACE_OUTER_BOUND ( 'NONE', #12140, .T. ) ;
#5833 = DIRECTION ( 'NONE',  ( -1.000000000000000000, -1.201369187114119994E-15, -9.616040805000176517E-16 ) ) ;
#5834 = ADVANCED_FACE ( 'NONE', ( #3925 ), #9953, .T. ) ;
#5835 =( BOUNDED_CURVE ( )  B_SPLINE_CURVE ( 3, ( #14763, #8011, #844, #9089 ),
 .UNSPECIFIED., .F., .T. ) 
 B_SPLINE_CURVE_WITH_KNOTS ( ( 4, 4 ),
 ( 5.266983419591685589, 7.299387194767492204 ),
 .UNSPECIFIED. ) 
 CURVE ( )  GEOMETRIC_REPRESENTATION_ITEM ( )  RATIONAL_B_SPLINE_CURVE ( ( 1.000000000000000000, 0.6843990470536787107, 0.6843990470536787107, 1.000000000000000000 ) ) 
 REPRESENTATION_ITEM ( '' )  );
#5836 = CARTESIAN_POINT ( 'NONE',  ( -7.730209135540895282, -46.40248289166846973, 22.00066548116162224 ) ) ;
#5838 = CARTESIAN_POINT ( 'NONE',  ( -38.49964551292070070, 3.992621007561997892, 24.26206422150100650 ) ) ;
#5837 = DIRECTION ( 'NONE',  ( 1.445602896647339656E-16, 0.000000000000000000, -1.000000000000000000 ) ) ;
#5839 = VERTEX_POINT ( 'NONE', #14479 ) ;
#5840 = FACE_OUTER_BOUND ( 'NONE', #10239, .T. ) ;
#5841 = DIRECTION ( 'NONE',  ( 0.000000000000000000, 1.000000000000000000, 1.224646799147350002E-16 ) ) ;
#5842 = ORIENTED_EDGE ( 'NONE', *, *, #7991, .T. ) ;
#5843 = AXIS2_PLACEMENT_3D ( 'NONE', #10762, #12065, #3873 ) ;
#5844 = VERTEX_POINT ( 'NONE', #14555 ) ;
#5845 = DIRECTION ( 'NONE',  ( -8.018662683283438208E-16, 5.975035461963189015E-16, 1.000000000000000000 ) ) ;
#5846 = CARTESIAN_POINT ( 'NONE',  ( -20.78589391471635039, -38.48009039869666736, 56.62973181049755311 ) ) ;
#5847 = VERTEX_POINT ( 'NONE', #414 ) ;
#5848 = VERTEX_POINT ( 'NONE', #6284 ) ;
#5849 = CARTESIAN_POINT ( 'NONE',  ( -15.49969986081099904, -37.00737899243799944, 19.50231026484399877 ) ) ;
#5850 = EDGE_CURVE ( 'NONE', #13612, #3714, #8580, .T. ) ;
#5851 = CARTESIAN_POINT ( 'NONE',  ( -13.97717856230794631, -23.42060321925418265, 56.97738585718026627 ) ) ;
#5852 = CARTESIAN_POINT ( 'NONE',  ( -33.49969986081099904, -51.00737899243799944, -13.39525803434800011 ) ) ;
#5853 = CARTESIAN_POINT ( 'NONE',  ( -9.508527451665001351, -44.50737899243799944, -5.497689735156000346 ) ) ;
#5854 = EDGE_CURVE ( 'NONE', #569, #10290, #8835, .T. ) ;
#5856 = VERTEX_POINT ( 'NONE', #7585 ) ;
#5855 = AXIS2_PLACEMENT_3D ( 'NONE', #4074, #8584, #8811 ) ;
#5857 = CARTESIAN_POINT ( 'NONE',  ( -10.32306602483566316, -90.56413277834681708, -4.064149291360593885 ) ) ;
#5858 = FACE_OUTER_BOUND ( 'NONE', #13373, .T. ) ;
#5859 = ORIENTED_EDGE ( 'NONE', *, *, #14030, .F. ) ;
#5860 = PLANE ( 'NONE',  #9983 ) ;
#5861 = VERTEX_POINT ( 'NONE', #12111 ) ;
#5862 = CARTESIAN_POINT ( 'NONE',  ( -15.49969986081099371, -36.50737899243799944, -17.99768973515599768 ) ) ;
#5863 = ORIENTED_EDGE ( 'NONE', *, *, #9359, .F. ) ;
#5864 = LINE ( 'NONE', #8010, #12285 ) ;
#5865 = FACE_BOUND ( 'NONE', #5600, .T. ) ;
#5866 = DIRECTION ( 'NONE',  ( 0.9826409426582659590, -0.1855175943453191700, 8.987940462991681405E-16 ) ) ;
#5867 = CARTESIAN_POINT ( 'NONE',  ( -8.005749619258239136, -47.31205335750601648, 46.87470529982511636 ) ) ;
#5868 = EDGE_CURVE ( 'NONE', #10153, #5342, #10548, .T. ) ;
#5869 = DIRECTION ( 'NONE',  ( -8.018662683283439195E-16, 5.975035461963190001E-16, 1.000000000000000000 ) ) ;
#5870 = EDGE_CURVE ( 'NONE', #13194, #4806, #7842, .T. ) ;
#5871 = CARTESIAN_POINT ( 'NONE',  ( -7.594860258898399330, -10.18326093375929631, 56.85231026484400019 ) ) ;
#5872 = ADVANCED_FACE ( 'NONE', ( #14407 ), #489, .F. ) ;
#5873 = CARTESIAN_POINT ( 'NONE',  ( -7.671650320578205395, -48.38766871647334966, -7.145439208203410608 ) ) ;
#5874 = CARTESIAN_POINT ( 'NONE',  ( -34.90864537991240724, -38.51142663665533661, 51.59020252618820024 ) ) ;
#5875 = AXIS2_PLACEMENT_3D ( 'NONE', #6360, #640, #11267 ) ;
#5876 = DIRECTION ( 'NONE',  ( 0.5975035461963189576, 0.8018662683283437342, 0.000000000000000000 ) ) ;
#5877 = ORIENTED_EDGE ( 'NONE', *, *, #8872, .T. ) ;
#5878 = CARTESIAN_POINT ( 'NONE',  ( 7.498862047384196927, 3.992621007561999669, 23.52554352489782730 ) ) ;
#5879 = ORIENTED_EDGE ( 'NONE', *, *, #3883, .T. ) ;
#5881 = EDGE_LOOP ( 'NONE', ( #2602, #485, #4528, #11008, #11483, #11337 ) ) ;
#5880 = CARTESIAN_POINT ( 'NONE',  ( -5.499699860811003482, -46.50737899243799944, 41.50231026484399166 ) ) ;
#5882 = EDGE_CURVE ( 'NONE', #6735, #2509, #1267, .T. ) ;
#5883 = VERTEX_POINT ( 'NONE', #14628 ) ;
#5884 = CARTESIAN_POINT ( 'NONE',  ( -15.49969986081099727, -107.2547982693967583, -7.854504911766861497 ) ) ;
#5885 = ORIENTED_EDGE ( 'NONE', *, *, #9474, .T. ) ;
#5886 = DIRECTION ( 'NONE',  ( 0.3857661296576204712, 0.9225966037272086417, -2.419218955996629202E-16 ) ) ;
#5887 = CARTESIAN_POINT ( 'NONE',  ( -20.84918524500973191, -107.1622034095862972, -5.012689735156006243 ) ) ;
#5888 = AXIS2_PLACEMENT_3D ( 'NONE', #8437, #13823, #13970 ) ;
#5889 = FACE_OUTER_BOUND ( 'NONE', #48, .T. ) ;
#5890 =( NAMED_UNIT ( * ) PLANE_ANGLE_UNIT ( ) SI_UNIT ( $, .RADIAN. ) );
#5891 = EDGE_CURVE ( 'NONE', #10757, #2844, #2491, .T. ) ;
#5892 = CARTESIAN_POINT ( 'NONE',  ( -18.24212484032476667, -9.927510438464585363, -13.18832502026138620 ) ) ;
#5893 = CARTESIAN_POINT ( 'NONE',  ( -24.32830346761242879, -18.15026423267100597, 54.00231026484399166 ) ) ;
#5894 = DIRECTION ( 'NONE',  ( -8.018662683283438208E-16, 5.975035461963189015E-16, 1.000000000000000000 ) ) ;
#5895 = AXIS2_PLACEMENT_3D ( 'NONE', #12336, #1778, #5076 ) ;
#5896 = ORIENTED_EDGE ( 'NONE', *, *, #10858, .F. ) ;
#5897 = FACE_OUTER_BOUND ( 'NONE', #14025, .T. ) ;
#5898 = ORIENTED_EDGE ( 'NONE', *, *, #6711, .F. ) ;
#5899 = VERTEX_POINT ( 'NONE', #3999 ) ;
#5900 = VERTEX_POINT ( 'NONE', #12261 ) ;
#5901 = AXIS2_PLACEMENT_3D ( 'NONE', #13337, #7347, #13262 ) ;
#5902 = CARTESIAN_POINT ( 'NONE',  ( 5.644331944133275769, -37.36437517128688057, 50.47299701629476942 ) ) ;
#5903 = VERTEX_POINT ( 'NONE', #7507 ) ;
#5905 = EDGE_CURVE ( 'NONE', #9600, #1021, #12039, .T. ) ;
#5904 = DIRECTION ( 'NONE',  ( -1.000000000000000000, 0.000000000000000000, 0.000000000000000000 ) ) ;
#5906 = FACE_OUTER_BOUND ( 'NONE', #2237, .T. ) ;
#5907 = VECTOR ( 'NONE', #14665, 1000.000000000000227 ) ;
#5908 = CARTESIAN_POINT ( 'NONE',  ( -11.97891935325373147, -91.04984766112443140, -9.554806339755154809 ) ) ;
#5909 = CIRCLE ( 'NONE', #14712, 3.249999999999999556 ) ;
#5910 = AXIS2_PLACEMENT_3D ( 'NONE', #5623, #11370, #8989 ) ;
#5911 = VECTOR ( 'NONE', #2217, 1000.000000000000000 ) ;
#5912 = CARTESIAN_POINT ( 'NONE',  ( -14.61203582817000068, -106.5081018427098201, -6.912624477443467974 ) ) ;
#5914 = CARTESIAN_POINT ( 'NONE',  ( 13.85920135429429934, -27.00737899243800300, 43.21206422150100224 ) ) ;
#5913 = CARTESIAN_POINT ( 'NONE',  ( -7.570456978157269035, -48.78587553030465784, -4.456442176039379532 ) ) ;
#5915 = ORIENTED_EDGE ( 'NONE', *, *, #13423, .T. ) ;
#5916 = DIRECTION ( 'NONE',  ( 0.5975035461963189576, 0.8018662683283437342, 0.000000000000000000 ) ) ;
#5917 = CARTESIAN_POINT ( 'NONE',  ( -15.64858178355719964, -107.0784156655072508, -4.488924337614155213 ) ) ;
#5918 = ORIENTED_EDGE ( 'NONE', *, *, #7662, .F. ) ;
#5919 = EDGE_LOOP ( 'NONE', ( #7562, #8899, #13932, #9486 ) ) ;
#5920 = CARTESIAN_POINT ( 'NONE',  ( 21.99848181214818155, -30.23659088485334934, 24.63578152807335897 ) ) ;
#5921 = CARTESIAN_POINT ( 'NONE',  ( -22.98851422383178544, -41.68127855727117748, 56.24708203345880975 ) ) ;
#5922 = ORIENTED_EDGE ( 'NONE', *, *, #8588, .F. ) ;
#5923 = CIRCLE ( 'NONE', #10573, 23.00000000000000000 ) ;
#5924 = FILL_AREA_STYLE ('',( #1427 ) ) ;
#5925 = VERTEX_POINT ( 'NONE', #5144 ) ;
#5926 = EDGE_CURVE ( 'NONE', #5586, #12315, #8806, .T. ) ;
#5927 = AXIS2_PLACEMENT_3D ( 'NONE', #14920, #9098, #11622 ) ;
#5928 = DIRECTION ( 'NONE',  ( 0.5975035461963189576, 0.8018662683283437342, 0.000000000000000000 ) ) ;
#5929 = LINE ( 'NONE', #59, #8245 ) ;
#5930 = AXIS2_PLACEMENT_3D ( 'NONE', #10488, #14998, #931 ) ;
#5931 = PLANE ( 'NONE',  #8198 ) ;
#5932 = CARTESIAN_POINT ( 'NONE',  ( -33.43612459426397265, 11.05255549920671321, 32.21545598376612674 ) ) ;
#5933 = ORIENTED_EDGE ( 'NONE', *, *, #12891, .T. ) ;
#5934 = CIRCLE ( 'NONE', #1804, 3.000000000000000000 ) ;
#5935 = CARTESIAN_POINT ( 'NONE',  ( -23.12048770254168062, -16.17743848078839619, 56.85231026484398598 ) ) ;
#5936 = CIRCLE ( 'NONE', #1312, 23.00000000000000000 ) ;
#5937 = CARTESIAN_POINT ( 'NONE',  ( -20.52642601085533869, -22.12321610861327770, 54.00231026484399166 ) ) ;
#5938 = ORIENTED_EDGE ( 'NONE', *, *, #14024, .T. ) ;
#5939 = CARTESIAN_POINT ( 'NONE',  ( -10.08476707729037614, -21.88467736064467672, 57.00231026484399166 ) ) ;
#5940 = ORIENTED_EDGE ( 'NONE', *, *, #3387, .T. ) ;
#5941 = CARTESIAN_POINT ( 'NONE',  ( -13.41639018438039699, -15.05973874201012741, 51.00231026484399166 ) ) ;
#5942 = EDGE_LOOP ( 'NONE', ( #4538, #4915, #13118, #13574 ) ) ;
#5943 = EDGE_CURVE ( 'NONE', #7946, #645, #12758, .T. ) ;
#5944 = PLANE ( 'NONE',  #12032 ) ;
#5945 = DIRECTION ( 'NONE',  ( -0.4491835085186243748, -0.8934395198752397294, 1.736481776669299976E-16 ) ) ;
#5946 = DIRECTION ( 'NONE',  ( 0.8222303661035966771, -0.5691548339926011391, 9.993908270190953088E-16 ) ) ;
#5947 = AXIS2_PLACEMENT_3D ( 'NONE', #2510, #3808, #11758 ) ;
#5948 = FACE_BOUND ( 'NONE', #2484, .T. ) ;
#5949 = CARTESIAN_POINT ( 'NONE',  ( -7.497885806132468467, -44.50611869254105102, 18.00659976627173720 ) ) ;
#5950 = FACE_OUTER_BOUND ( 'NONE', #14101, .T. ) ;
#5951 = VECTOR ( 'NONE', #2206, 1000.000000000000000 ) ;
#5952 = LINE ( 'NONE', #9323, #3576 ) ;
#5953 = ORIENTED_EDGE ( 'NONE', *, *, #3986, .T. ) ;
#5954 = DIRECTION ( 'NONE',  ( 0.000000000000000000, 0.1872998510044759646, 0.9823027872370621028 ) ) ;
#5955 = DIRECTION ( 'NONE',  ( -0.5401126942952620968, -0.8415927028326188886, 6.975647374412522208E-17 ) ) ;
#5956 = CIRCLE ( 'NONE', #10355, 10.00000000000000000 ) ;
#5957 = CARTESIAN_POINT ( 'NONE',  ( -23.49969986081099904, -44.50737899243799944, -5.497689735156002122 ) ) ;
#5958 = ORIENTED_EDGE ( 'NONE', *, *, #723, .F. ) ;
#5959 = DIRECTION ( 'NONE',  ( -0.4177292884839868270, -0.9085715390340278752, 2.079116908177700458E-16 ) ) ;
#5960 = VERTEX_POINT ( 'NONE', #1701 ) ;
#5962 = ORIENTED_EDGE ( 'NONE', *, *, #2963, .F. ) ;
#5961 = DIRECTION ( 'NONE',  ( -8.018662683283438208E-16, 5.975035461963189015E-16, 1.000000000000000000 ) ) ;
#5963 = ORIENTED_EDGE ( 'NONE', *, *, #14486, .F. ) ;
#5964 = ADVANCED_FACE ( 'NONE', ( #6354 ), #11029, .T. ) ;
#5965 = CARTESIAN_POINT ( 'NONE',  ( -12.04767799572592502, -20.80732214584531548, 56.85231026484400019 ) ) ;
#5966 = ORIENTED_EDGE ( 'NONE', *, *, #13391, .F. ) ;
#5967 = AXIS2_PLACEMENT_3D ( 'NONE', #2560, #7209, #11889 ) ;
#5968 = CARTESIAN_POINT ( 'NONE',  ( -16.32149003149046607, -5.473954385499126829, 56.85231026484398598 ) ) ;
#5969 = ADVANCED_FACE ( 'NONE', ( #5663 ), #10334, .F. ) ;
#5970 = CARTESIAN_POINT ( 'NONE',  ( -14.00164528647249007, -5.572553380472728968, 56.85231026484398598 ) ) ;
#5971 = VECTOR ( 'NONE', #3093, 1000.000000000000114 ) ;
#5972 = DIRECTION ( 'NONE',  ( 0.000000000000000000, 0.000000000000000000, 1.000000000000000000 ) ) ;
#5973 = CARTESIAN_POINT ( 'NONE',  ( 0.000000000000000000, 0.000000000000000000, 0.000000000000000000 ) ) ;
#5974 = ADVANCED_FACE ( 'NONE', ( #7953 ), #5369, .F. ) ;
#5975 = CARTESIAN_POINT ( 'NONE',  ( -18.26066734922995494, -14.69693585872053632, 57.00231026484398456 ) ) ;
#5976 = DIRECTION ( 'NONE',  ( -1.000000000000000000, -1.201369187114119994E-15, -9.616040805000176517E-16 ) ) ;
#5977 = CARTESIAN_POINT ( 'NONE',  ( 13.85920135429429934, -27.00737899243800300, 2.712064221501000461 ) ) ;
#5978 = CARTESIAN_POINT ( 'NONE',  ( 4.376462137075568748, -38.10176464241877881, -12.29701886598900806 ) ) ;
#5979 = ORIENTED_EDGE ( 'NONE', *, *, #5228, .T. ) ;
#5980 = ORIENTED_EDGE ( 'NONE', *, *, #13810, .F. ) ;
#5981 = VERTEX_POINT ( 'NONE', #2160 ) ;
#5982 = AXIS2_PLACEMENT_3D ( 'NONE', #14170, #2538, #14087 ) ;
#5983 = EDGE_CURVE ( 'NONE', #5192, #5306, #2634, .T. ) ;
#5984 = DIRECTION ( 'NONE',  ( -0.1272150336605082366, 0.9918751611018171710, -6.946583704589972670E-16 ) ) ;
#5985 = EDGE_CURVE ( 'NONE', #1451, #9234, #1409, .T. ) ;
#5986 = ORIENTED_EDGE ( 'NONE', *, *, #1585, .F. ) ;
#5987 = DIRECTION ( 'NONE',  ( -1.000000000000000000, 0.000000000000000000, 0.000000000000000000 ) ) ;
#5988 = DIRECTION ( 'NONE',  ( -0.09252159378507134047, 0.9957106782009873536, -6.691306063588577540E-16 ) ) ;
#5989 = CARTESIAN_POINT ( 'NONE',  ( 9.000300139189000959, -27.00737899243800300, 5.212064221501000461 ) ) ;
#5991 = CARTESIAN_POINT ( 'NONE',  ( -22.64031343690345111, -17.27870339600297811, 57.00231026484397745 ) ) ;
#5990 = DIRECTION ( 'NONE',  ( 0.000000000000000000, 0.1872998510044689147, 0.9823027872370635460 ) ) ;
#5992 = ORIENTED_EDGE ( 'NONE', *, *, #13827, .T. ) ;
#5993 = DIRECTION ( 'NONE',  ( 3.632077277826439854E-16, -1.000000000000000000, 0.000000000000000000 ) ) ;
#5994 = CARTESIAN_POINT ( 'NONE',  ( -24.59223421123983400, -17.67354377200967264, 60.59320803929022503 ) ) ;
#5995 = ORIENTED_EDGE ( 'NONE', *, *, #7360, .T. ) ;
#5996 = ORIENTED_EDGE ( 'NONE', *, *, #4675, .T. ) ;
#5997 = CARTESIAN_POINT ( 'NONE',  ( -21.68801466096620700, -19.44379288755867208, 57.00231026484397745 ) ) ;
#5998 = EDGE_CURVE ( 'NONE', #8595, #13469, #5589, .T. ) ;
#5999 = ORIENTED_EDGE ( 'NONE', *, *, #13101, .T. ) ;
#6000 = CARTESIAN_POINT ( 'NONE',  ( -24.55043086433169819, -12.83990741858047357, 56.85231026484398598 ) ) ;
#6001 = AXIS2_PLACEMENT_3D ( 'NONE', #4013, #11271, #12497 ) ;
#6002 = AXIS2_PLACEMENT_3D ( 'NONE', #10302, #4801, #4883 ) ;
#6003 = DIRECTION ( 'NONE',  ( 1.000000000000000000, 1.201369187114119994E-15, 9.616040805000176517E-16 ) ) ;
#6004 = EDGE_CURVE ( 'NONE', #11664, #10889, #9719, .T. ) ;
#6005 = CARTESIAN_POINT ( 'NONE',  ( -23.02734322232803521, -10.58405290357860373, 57.00231026484397745 ) ) ;
#6006 = CARTESIAN_POINT ( 'NONE',  ( -23.49969986081099904, -44.50737899243799944, 19.50231026484399877 ) ) ;
#6007 = VERTEX_POINT ( 'NONE', #11486 ) ;
#6008 = CARTESIAN_POINT ( 'NONE',  ( -2.216578225681298697, -31.14135358865360104, 59.28069236156870403 ) ) ;
#6009 = LINE ( 'NONE', #8465, #8229 ) ;
#6010 = VERTEX_POINT ( 'NONE', #13787 ) ;
#6011 = LINE ( 'NONE', #9619, #7375 ) ;
#6012 = ORIENTED_EDGE ( 'NONE', *, *, #936, .T. ) ;
#6013 = DIRECTION ( 'NONE',  ( 9.912705577010322591E-16, -0.1872998510044552312, -0.9823027872370662106 ) ) ;
#6014 = ORIENTED_EDGE ( 'NONE', *, *, #11526, .F. ) ;
#6015 = CARTESIAN_POINT ( 'NONE',  ( -15.42469986081099442, -23.50737899243800300, 56.85231026484400019 ) ) ;
#6016 = PLANE ( 'NONE',  #12665 ) ;
#6017 = CARTESIAN_POINT ( 'NONE',  ( -15.10625462230756177, -3.540141368888813922, 56.85231026484398598 ) ) ;
#6018 = AXIS2_PLACEMENT_3D ( 'NONE', #1976, #9998, #13530 ) ;
#6019 = CARTESIAN_POINT ( 'NONE',  ( -6.097673344397686712, -16.91980966733272140, 60.51440242979897022 ) ) ;
#6020 = ADVANCED_FACE ( 'NONE', ( #1928 ), #13627, .T. ) ;
#6021 = CARTESIAN_POINT ( 'NONE',  ( 22.00030013918900096, -27.00737899243800300, 45.71206422150100224 ) ) ;
#6022 = VERTEX_POINT ( 'NONE', #4378 ) ;
#6023 = DIRECTION ( 'NONE',  ( 8.018662683283438208E-16, -5.975035461963189015E-16, -1.000000000000000000 ) ) ;
#6024 = DIRECTION ( 'NONE',  ( 0.000000000000000000, 0.1872998510044689147, 0.9823027872370635460 ) ) ;
#6025 = LINE ( 'NONE', #14308, #821 ) ;
#6026 = EDGE_LOOP ( 'NONE', ( #1636, #12125, #9968, #5199 ) ) ;
#6027 = CARTESIAN_POINT ( 'NONE',  ( -13.57551609484869815, -3.719726473329904248, 56.85231026484398598 ) ) ;
#6028 = ORIENTED_EDGE ( 'NONE', *, *, #15077, .F. ) ;
#6029 = VECTOR ( 'NONE', #1580, 1000.000000000000000 ) ;
#6031 = ORIENTED_EDGE ( 'NONE', *, *, #9382, .T. ) ;
#6030 = CARTESIAN_POINT ( 'NONE',  ( -33.49969986081094220, -41.82625798754038016, -13.39525803434798412 ) ) ;
#6032 = EDGE_LOOP ( 'NONE', ( #4463, #8968, #14331, #3146 ) ) ;
#6033 = FACE_OUTER_BOUND ( 'NONE', #3777, .T. ) ;
#6034 = CIRCLE ( 'NONE', #8974, 0.2000000000000012046 ) ;
#6035 = CARTESIAN_POINT ( 'NONE',  ( -14.00594099532011860, -11.50271332161736915, 51.25231026484399166 ) ) ;
#6036 = ORIENTED_EDGE ( 'NONE', *, *, #9823, .F. ) ;
#6037 = CARTESIAN_POINT ( 'NONE',  ( -14.76203582816999926, -107.4899781488447985, -7.806719612820866239 ) ) ;
#6038 = DIRECTION ( 'NONE',  ( 0.3204693369899919708, 0.9472588896649083434, -3.090169943749469383E-16 ) ) ;
#6039 = CARTESIAN_POINT ( 'NONE',  ( -15.61203582816999713, -107.9151965264422586, -6.615812085103269347 ) ) ;
#6040 =( NAMED_UNIT ( * ) SI_UNIT ( $, .STERADIAN. ) SOLID_ANGLE_UNIT ( ) );
#6041 = AXIS2_PLACEMENT_3D ( 'NONE', #7058, #11736, #128 ) ;
#6042 = CARTESIAN_POINT ( 'NONE',  ( -15.49969986081099371, -9.007378992438001220, -13.28793577849899599 ) ) ;
#6043 = EDGE_CURVE ( 'NONE', #8709, #2126, #4197, .T. ) ;
#6044 = AXIS2_PLACEMENT_3D ( 'NONE', #3765, #3535, #7193 ) ;
#6045 = FACE_OUTER_BOUND ( 'NONE', #10448, .T. ) ;
#6046 = EDGE_CURVE ( 'NONE', #3379, #6794, #5752, .T. ) ;
#6047 = CARTESIAN_POINT ( 'NONE',  ( 2.500300139188999182, -42.00737899243800655, -13.39525803434800011 ) ) ;
#6048 = EDGE_LOOP ( 'NONE', ( #8393, #7180, #161, #8935 ) ) ;
#6049 = EDGE_LOOP ( 'NONE', ( #11044, #5093, #7776, #13991 ) ) ;
#6050 = ORIENTED_EDGE ( 'NONE', *, *, #7206, .T. ) ;
#6051 = CARTESIAN_POINT ( 'NONE',  ( -20.39403028972282428, -7.084672814149619136, 57.00231026484397745 ) ) ;
#6052 = ORIENTED_EDGE ( 'NONE', *, *, #266, .F. ) ;
#6053 = VECTOR ( 'NONE', #925, 1000.000000000000000 ) ;
#6054 = LINE ( 'NONE', #1482, #10040 ) ;
#6055 = DIRECTION ( 'NONE',  ( -0.7805252200231683757, 0.6251242923673537843, -9.993908270190959005E-16 ) ) ;
#6056 = CIRCLE ( 'NONE', #1432, 37.50000000000000000 ) ;
#6057 = EDGE_CURVE ( 'NONE', #4202, #6280, #11186, .T. ) ;
#6058 = CYLINDRICAL_SURFACE ( 'NONE', #11985, 9.974999999999997868 ) ;
#6059 = CARTESIAN_POINT ( 'NONE',  ( -6.507973901336479017, -12.27851192488648024, 56.85231026484400019 ) ) ;
#6060 = ADVANCED_FACE ( 'NONE', ( #2082 ), #11407, .F. ) ;
#6061 = EDGE_CURVE ( 'NONE', #12214, #2702, #11139, .T. ) ;
#6062 = DIRECTION ( 'NONE',  ( 0.5975035461963188466, 0.8018662683283437342, 0.000000000000000000 ) ) ;
#6064 = DIRECTION ( 'NONE',  ( 0.7582332219680881780, -0.6519834208811539078, 9.975640502598240034E-16 ) ) ;
#6063 = CARTESIAN_POINT ( 'NONE',  ( -7.526618194427104669, -48.92257192762266271, -6.159325076304092761 ) ) ;
#6065 = ORIENTED_EDGE ( 'NONE', *, *, #8421, .F. ) ;
#6066 = LINE ( 'NONE', #2639, #10698 ) ;
#6067 = DIRECTION ( 'NONE',  ( 1.000000000000000000, 1.000000000000000078E-15, 0.000000000000000000 ) ) ;
#6068 = ORIENTED_EDGE ( 'NONE', *, *, #4870, .F. ) ;
#6069 = ORIENTED_EDGE ( 'NONE', *, *, #5012, .T. ) ;
#6070 = CARTESIAN_POINT ( 'NONE',  ( 21.99843046478421371, -30.23599839927906530, 23.78383503728017345 ) ) ;
#6071 = DIRECTION ( 'NONE',  ( 8.018662683283438208E-16, -5.975035461963189015E-16, -1.000000000000000000 ) ) ;
#6072 = ORIENTED_EDGE ( 'NONE', *, *, #14196, .T. ) ;
#6073 = VECTOR ( 'NONE', #411, 1000.000000000000000 ) ;
#6074 = CARTESIAN_POINT ( 'NONE',  ( -12.91616447596942230, -36.91800560015940391, -17.91172472810691119 ) ) ;
#6075 = ADVANCED_FACE ( 'NONE', ( #4298 ), #13632, .T. ) ;
#6076 = DIRECTION ( 'NONE',  ( 0.000000000000000000, 1.000000000000000000, 1.224646799147350002E-16 ) ) ;
#6077 = CARTESIAN_POINT ( 'NONE',  ( 22.00030013918900096, -27.00737899243800300, 43.21206422150100224 ) ) ;
#6078 = EDGE_CURVE ( 'NONE', #2929, #11933, #6653, .T. ) ;
#6079 = VECTOR ( 'NONE', #10413, 1000.000000000000000 ) ;
#6080 = AXIS2_PLACEMENT_3D ( 'NONE', #13752, #900, #1050 ) ;
#6081 = CARTESIAN_POINT ( 'NONE',  ( -15.49969986081092088, -110.0073789924380065, -0.1262635860074601546 ) ) ;
#6082 = DIRECTION ( 'NONE',  ( 0.000000000000000000, -1.000000000000000000, -1.224646799147350002E-16 ) ) ;
#6083 = ORIENTED_EDGE ( 'NONE', *, *, #5377, .T. ) ;
#6084 = CARTESIAN_POINT ( 'NONE',  ( -9.401538680480957311, -6.786242167561306715, 57.00231026484397745 ) ) ;
#6085 = PLANE ( 'NONE',  #10679 ) ;
#6086 = ORIENTED_EDGE ( 'NONE', *, *, #1688, .F. ) ;
#6087 = CARTESIAN_POINT ( 'NONE',  ( -15.49969986081099904, 71.39262100756199914, 24.21206422150100579 ) ) ;
#6088 = FILL_AREA_STYLE ('',( #14369 ) ) ;
#6089 = ORIENTED_EDGE ( 'NONE', *, *, #8226, .F. ) ;
#6090 = DIRECTION ( 'NONE',  ( -8.018662683283439195E-16, 5.975035461963190001E-16, 1.000000000000000000 ) ) ;
#6091 = ORIENTED_EDGE ( 'NONE', *, *, #1314, .T. ) ;
#6092 = DIRECTION ( 'NONE',  ( 9.804908406240741039E-16, -0.05233595624294555548, -0.9986295347545738332 ) ) ;
#6093 = EDGE_CURVE ( 'NONE', #14313, #5899, #7748, .T. ) ;
#6094 = CARTESIAN_POINT ( 'NONE',  ( -35.18530787408279537, 11.99262100756689620, 16.16206422150100153 ) ) ;
#6095 = DIRECTION ( 'NONE',  ( -8.018662683283438208E-16, 5.975035461963189015E-16, 1.000000000000000000 ) ) ;
#6096 =( GEOMETRIC_REPRESENTATION_CONTEXT ( 3 ) GLOBAL_UNCERTAINTY_ASSIGNED_CONTEXT ( ( #4326 ) ) GLOBAL_UNIT_ASSIGNED_CONTEXT ( ( #4858, #10662, #12045 ) ) REPRESENTATION_CONTEXT ( 'NONE', 'WORKASPACE' ) );
#6097 = DIRECTION ( 'NONE',  ( -0.3204693369899910826, -0.9472588896649086765, 3.090169943749478258E-16 ) ) ;
#6098 = ORIENTED_EDGE ( 'NONE', *, *, #12649, .F. ) ;
#6099 = LINE ( 'NONE', #13089, #8476 ) ;
#6100 = CARTESIAN_POINT ( 'NONE',  ( -15.49969986081099194, -57.00737899243800655, 19.50231026484399521 ) ) ;
#6101 = FACE_OUTER_BOUND ( 'NONE', #10524, .T. ) ;
#6102 = ORIENTED_EDGE ( 'NONE', *, *, #73, .T. ) ;
#6103 = CARTESIAN_POINT ( 'NONE',  ( -7.510312366833470143, -44.09314884015893199, -4.806344695767887920 ) ) ;
#6104 = ORIENTED_EDGE ( 'NONE', *, *, #4578, .T. ) ;
#6106 = VERTEX_POINT ( 'NONE', #8261 ) ;
#6105 = CARTESIAN_POINT ( 'NONE',  ( -24.88854884048805616, -16.87637585156647546, 54.00231026484397745 ) ) ;
#6107 = ORIENTED_EDGE ( 'NONE', *, *, #9731, .F. ) ;
#6108 = VECTOR ( 'NONE', #9726, 999.9999999999998863 ) ;
#6109 = PLANE ( 'NONE',  #4706 ) ;
#6110 = EDGE_LOOP ( 'NONE', ( #2830, #10989, #7686, #12237 ) ) ;
#6111 = DIRECTION ( 'NONE',  ( 0.5975035461963189576, 0.8018662683283437342, 0.000000000000000000 ) ) ;
#6112 = ADVANCED_FACE ( 'NONE', ( #7104 ), #3450, .T. ) ;
#6113 = PLANE ( 'NONE',  #13087 ) ;
#6114 = CARTESIAN_POINT ( 'NONE',  ( -15.49969986081092088, -13.50737899243822504, 56.85231026484398598 ) ) ;
#6115 =( NAMED_UNIT ( * ) PLANE_ANGLE_UNIT ( ) SI_UNIT ( $, .RADIAN. ) );
#6116 = CARTESIAN_POINT ( 'NONE',  ( -7.499849062438288527, -12.40572695854698360, 57.00231026484399166 ) ) ;
#6117 = DIRECTION ( 'NONE',  ( 1.000000000000000000, 1.201369187114119994E-15, 9.616040805000176517E-16 ) ) ;
#6118 = CARTESIAN_POINT ( 'NONE',  ( -11.02913861065588641, -14.09954045717994653, -13.02054842795066314 ) ) ;
#6119 = EDGE_LOOP ( 'NONE', ( #11961, #1997, #3398, #13963, #4599, #130, #12350, #9737, #9565, #10862, #4927, #2344, #12671, #3886, #12123, #2974, #1969 ) ) ;
#6120 = CARTESIAN_POINT ( 'NONE',  ( -15.61203582816999891, -108.4210244314312916, -5.847664976093792433 ) ) ;
#6121 = FILL_AREA_STYLE_COLOUR ( '', #9451 ) ;
#6122 = ORIENTED_EDGE ( 'NONE', *, *, #10829, .F. ) ;
#6123 = EDGE_LOOP ( 'NONE', ( #10353, #15079, #5863, #14811 ) ) ;
#6124 = CARTESIAN_POINT ( 'NONE',  ( -15.49969986081099904, 9.919219809770901009, 5.212064221501000461 ) ) ;
#6125 = ORIENTED_EDGE ( 'NONE', *, *, #3838, .F. ) ;
#6126 = DIRECTION ( 'NONE',  ( 1.000000000000000000, 1.201369187114119994E-15, 9.616040805000176517E-16 ) ) ;
#6127 = VECTOR ( 'NONE', #1404, 1000.000000000000000 ) ;
#6128 = LINE ( 'NONE', #8438, #323 ) ;
#6129 = ADVANCED_FACE ( 'NONE', ( #10491 ), #19, .T. ) ;
#6130 = ADVANCED_FACE ( 'NONE', ( #5815 ), #11562, .F. ) ;
#6131 = DIRECTION ( 'NONE',  ( 8.018662683283438208E-16, -5.975035461963189015E-16, -1.000000000000000000 ) ) ;
#6132 = PLANE ( 'NONE',  #7286 ) ;
#6133 = CIRCLE ( 'NONE', #11531, 2.999999999999999112 ) ;
#6134 = AXIS2_PLACEMENT_3D ( 'NONE', #395, #10788, #6256 ) ;
#6135 = FACE_OUTER_BOUND ( 'NONE', #8462, .T. ) ;
#6137 = CARTESIAN_POINT ( 'NONE',  ( -7.887638505697306179, -19.95386229157006497, 56.85231026484400019 ) ) ;
#6136 = CARTESIAN_POINT ( 'NONE',  ( -7.513186133687160151, -48.97671528745701863, -5.011691156799132685 ) ) ;
#6138 = ORIENTED_EDGE ( 'NONE', *, *, #12527, .F. ) ;
#6139 = DIRECTION ( 'NONE',  ( -0.04695496274984587576, -0.9988970074402868660, 5.591929034707467802E-16 ) ) ;
#6140 = CYLINDRICAL_SURFACE ( 'NONE', #8687, 0.2499999999999996947 ) ;
#6141 = ORIENTED_EDGE ( 'NONE', *, *, #14356, .T. ) ;
#6142 = EDGE_LOOP ( 'NONE', ( #14512, #2401, #14405, #204 ) ) ;
#6143 = CARTESIAN_POINT ( 'NONE',  ( 21.97318612132534099, -29.92907000624635927, 25.65138358613589276 ) ) ;
#6144 = CARTESIAN_POINT ( 'NONE',  ( -6.424455519809837867, -13.54187755947681993, 57.00231026484399166 ) ) ;
#6145 = ORIENTED_EDGE ( 'NONE', *, *, #10015, .F. ) ;
#6146 = LINE ( 'NONE', #5370, #10856 ) ;
#6147 = EDGE_CURVE ( 'NONE', #2967, #1092, #4587, .T. ) ;
#6148 = VECTOR ( 'NONE', #12185, 1000.000000000000000 ) ;
#6149 = ADVANCED_FACE ( 'NONE', ( #8104 ), #2310, .T. ) ;
#6150 = VECTOR ( 'NONE', #6262, 999.9999999999998863 ) ;
#6151 = SHAPE_REPRESENTATION ( 'Tapered Toolholder Shank', ( #6789 ), #8750 ) ;
#6152 = VECTOR ( 'NONE', #4851, 1000.000000000000000 ) ;
#6153 = CIRCLE ( 'NONE', #8608, 9.974999999999999645 ) ;
#6154 = EDGE_CURVE ( 'NONE', #3452, #13092, #12652, .T. ) ;
#6155 = CARTESIAN_POINT ( 'NONE',  ( 7.444842330671914254, 4.142642748846463441, 25.83772173559120944 ) ) ;
#6156 = CARTESIAN_POINT ( 'NONE',  ( -18.09969986081099691, -109.8281559964656822, -5.947973080403810009 ) ) ;
#6157 = EDGE_CURVE ( 'NONE', #6428, #4722, #9335, .T. ) ;
#6158 = CARTESIAN_POINT ( 'NONE',  ( -7.497885806132468467, -44.50611869254105102, 18.00659976627173720 ) ) ;
#6159 = LINE ( 'NONE', #13301, #3500 ) ;
#6160 = ORIENTED_EDGE ( 'NONE', *, *, #3386, .F. ) ;
#6161 = LINE ( 'NONE', #1275, #10925 ) ;
#6162 = AXIS2_PLACEMENT_3D ( 'NONE', #119, #9435, #9666 ) ;
#6163 = DIRECTION ( 'NONE',  ( 1.000000000000000000, 0.000000000000000000, 0.000000000000000000 ) ) ;
#6164 = ORIENTED_EDGE ( 'NONE', *, *, #11866, .T. ) ;
#6165 = AXIS2_PLACEMENT_3D ( 'NONE', #6716, #5578, #14994 ) ;
#6166 = CARTESIAN_POINT ( 'NONE',  ( -7.497219220929387973, -44.39058125335130001, 18.15858026693495475 ) ) ;
#6167 =( NAMED_UNIT ( * ) SI_UNIT ( $, .STERADIAN. ) SOLID_ANGLE_UNIT ( ) );
#6168 = EDGE_LOOP ( 'NONE', ( #3601, #825, #4166, #1830 ) ) ;
#6169 = CARTESIAN_POINT ( 'NONE',  ( -14.61203582817000246, -106.3249253597797406, -5.117531130952052365 ) ) ;
#6170 = ORIENTED_EDGE ( 'NONE', *, *, #2073, .F. ) ;
#6171 = DIRECTION ( 'NONE',  ( 8.018662683283438208E-16, -5.975035461963189015E-16, -1.000000000000000000 ) ) ;
#6172 = EDGE_CURVE ( 'NONE', #186, #11757, #14242, .T. ) ;
#6173 = ADVANCED_FACE ( 'NONE', ( #8416 ), #11864, .T. ) ;
#6174 = PLANE ( 'NONE',  #14543 ) ;
#6175 = CARTESIAN_POINT ( 'NONE',  ( 13.85920135429429934, -27.00737899243800300, 43.21206422150100224 ) ) ;
#6176 = VECTOR ( 'NONE', #3066, 1000.000000000000227 ) ;
#6177 = CARTESIAN_POINT ( 'NONE',  ( 13.85920135429429934, -27.00737899243800300, 24.21206422150099868 ) ) ;
#6178 = AXIS2_PLACEMENT_3D ( 'NONE', #13070, #6082, #10841 ) ;
#6179 = CARTESIAN_POINT ( 'NONE',  ( 18.53245405280430802, -27.24065255069785252, 8.462064221501002237 ) ) ;
#6180 = ORIENTED_EDGE ( 'NONE', *, *, #8823, .F. ) ;
#6181 = CARTESIAN_POINT ( 'NONE',  ( -12.19394264074465895, -51.79708643885629726, -17.85247874086887165 ) ) ;
#6182 = CARTESIAN_POINT ( 'NONE',  ( -14.61203582817000246, -106.2173407584721616, -5.758565883178084377 ) ) ;
#6183 = ORIENTED_EDGE ( 'NONE', *, *, #6592, .F. ) ;
#6184 = CARTESIAN_POINT ( 'NONE',  ( 2.013526631810669265, 8.758714366253697037, 31.58011097299207037 ) ) ;
#6185 = EDGE_LOOP ( 'NONE', ( #9951, #2552, #14626, #14096 ) ) ;
#6187 = ORIENTED_EDGE ( 'NONE', *, *, #10998, .F. ) ;
#6186 = CARTESIAN_POINT ( 'NONE',  ( -15.45378054160984682, -13.48759475315262613, 56.85231026484398598 ) ) ;
#6188 = ORIENTED_EDGE ( 'NONE', *, *, #7905, .F. ) ;
#6189 = VECTOR ( 'NONE', #9161, 1000.000000000000114 ) ;
#6190 = DIRECTION ( 'NONE',  ( -8.018662683283438208E-16, 5.975035461963189015E-16, 1.000000000000000000 ) ) ;
#6191 = ORIENTED_EDGE ( 'NONE', *, *, #11136, .T. ) ;
#6192 = FACE_OUTER_BOUND ( 'NONE', #11819, .T. ) ;
#6193 = AXIS2_PLACEMENT_3D ( 'NONE', #8681, #4252, #9979 ) ;
#6194 = CARTESIAN_POINT ( 'NONE',  ( -23.41792317787242084, -15.09084496969942535, 57.00231026484397745 ) ) ;
#6195 = DIRECTION ( 'NONE',  ( 1.000000000000000000, 9.425792497760098106E-16, -9.335747894956348063E-17 ) ) ;
#6196 = DIRECTION ( 'NONE',  ( 0.4274949678123838859, -0.9040177279761104634, 8.829475928589268008E-16 ) ) ;
#6197 = AXIS2_PLACEMENT_3D ( 'NONE', #11825, #12987, #1350 ) ;
#6198 = EDGE_CURVE ( 'NONE', #6401, #11027, #1151, .T. ) ;
#6199 = ADVANCED_FACE ( 'NONE', ( #9492 ), #8184, .F. ) ;
#6200 = CARTESIAN_POINT ( 'NONE',  ( -8.744338604334316756, -15.61126689213601360, 57.00231026484399166 ) ) ;
#6201 = LINE ( 'NONE', #484, #8826 ) ;
#6202 = ORIENTED_EDGE ( 'NONE', *, *, #7898, .F. ) ;
#6203 = DIRECTION ( 'NONE',  ( -8.018662683283438208E-16, 5.975035461963189015E-16, 1.000000000000000000 ) ) ;
#6204 = VERTEX_POINT ( 'NONE', #7026 ) ;
#6205 = VERTEX_POINT ( 'NONE', #8339 ) ;
#6206 = DIRECTION ( 'NONE',  ( 8.018662683283438208E-16, -5.975035461963189015E-16, -1.000000000000000000 ) ) ;
#6207 = DIRECTION ( 'NONE',  ( 0.000000000000000000, -1.000000000000000000, -1.224646799147350002E-16 ) ) ;
#6208 = ORIENTED_EDGE ( 'NONE', *, *, #12370, .F. ) ;
#6209 = ORIENTED_EDGE ( 'NONE', *, *, #2972, .F. ) ;
#6210 = CYLINDRICAL_SURFACE ( 'NONE', #966, 0.2500000000000004441 ) ;
#6211 = AXIS2_PLACEMENT_3D ( 'NONE', #11081, #604, #9152 ) ;
#6212 = CARTESIAN_POINT ( 'NONE',  ( -15.49969986081099904, 70.81438635534659909, 24.21206422150100579 ) ) ;
#6213 = DIRECTION ( 'NONE',  ( 0.000000000000000000, 1.131341397376178572E-16, -1.000000000000000000 ) ) ;
#6214 = CARTESIAN_POINT ( 'NONE',  ( -15.45180655762527699, -13.52173975529984418, 56.85231026484398598 ) ) ;
#6215 = AXIS2_PLACEMENT_3D ( 'NONE', #8086, #78, #1069 ) ;
#6216 = EDGE_CURVE ( 'NONE', #2729, #13889, #10718, .T. ) ;
#6218 = CARTESIAN_POINT ( 'NONE',  ( -37.58940743239428173, 5.168430268690432428, 19.97516569973667089 ) ) ;
#6217 = CARTESIAN_POINT ( 'NONE',  ( -7.638565634192135079, -48.52246210453047581, -4.016914597510680807 ) ) ;
#6219 = VERTEX_POINT ( 'NONE', #10562 ) ;
#6220 = CARTESIAN_POINT ( 'NONE',  ( -15.49969986081099371, -52.50737899243799944, -17.99768973515599768 ) ) ;
#6221 = LINE ( 'NONE', #8448, #9363 ) ;
#6222 = VERTEX_POINT ( 'NONE', #4914 ) ;
#6223 = ORIENTED_EDGE ( 'NONE', *, *, #12788, .T. ) ;
#6224 = CARTESIAN_POINT ( 'NONE',  ( -23.08909483861678069, -47.09084248276676732, 56.22686388828775961 ) ) ;
#6225 = ORIENTED_EDGE ( 'NONE', *, *, #14828, .F. ) ;
#6226 = DIRECTION ( 'NONE',  ( 0.000000000000000000, -1.000000000000000000, -1.224646799147350002E-16 ) ) ;
#6227 = DIRECTION ( 'NONE',  ( -0.3306575217771102193, 0.9437508163134058492, -8.290375725550400094E-16 ) ) ;
#6228 = DIRECTION ( 'NONE',  ( 0.6626200482157369454, 0.03919731383111578482, 0.7479293030032981848 ) ) ;
#6229 = EDGE_CURVE ( 'NONE', #1960, #11221, #94, .T. ) ;
#6230 = LINE ( 'NONE', #10684, #2041 ) ;
#6231 = ORIENTED_EDGE ( 'NONE', *, *, #12022, .F. ) ;
#6232 = CARTESIAN_POINT ( 'NONE',  ( -21.67659902633306146, -21.33978230808610022, 57.00231026484397745 ) ) ;
#6233 = VERTEX_POINT ( 'NONE', #4756 ) ;
#6234 = ADVANCED_FACE ( 'NONE', ( #2231 ), #6876, .F. ) ;
#6235 = CARTESIAN_POINT ( 'NONE',  ( 2.374542637206501272, 7.183219930803497633, 17.76912582958182085 ) ) ;
#6236 = DIRECTION ( 'NONE',  ( 0.9183863840214729901, 0.3956847857120157075, 4.999999999999999402E-16 ) ) ;
#6237 = ORIENTED_EDGE ( 'NONE', *, *, #6247, .F. ) ;
#6238 = AXIS2_PLACEMENT_3D ( 'NONE', #981, #3572, #11606 ) ;
#6239 = CARTESIAN_POINT ( 'NONE',  ( -29.57393575939416408, -54.93314309385483796, 54.32987364559346588 ) ) ;
#6240 = VERTEX_POINT ( 'NONE', #3493 ) ;
#6241 = CARTESIAN_POINT ( 'NONE',  ( 13.85920135429429934, -27.00737899243800300, 1.962064221501000683 ) ) ;
#6242 = FACE_OUTER_BOUND ( 'NONE', #12330, .T. ) ;
#6243 = CARTESIAN_POINT ( 'NONE',  ( -15.49969986081100082, -109.4746705577010744, -0.8002025553967917482 ) ) ;
#6244 = LINE ( 'NONE', #602, #8221 ) ;
#6245 = AXIS2_PLACEMENT_3D ( 'NONE', #13551, #13774, #11396 ) ;
#6246 = LINE ( 'NONE', #6021, #4541 ) ;
#6247 = EDGE_CURVE ( 'NONE', #13484, #1625, #5929, .T. ) ;
#6248 = B_SPLINE_CURVE_WITH_KNOTS ( 'NONE', 3,
 ( #6983, #10525, #2572, #3718, #8147, #3795, #8223, #8454, #3489, #8374, #9605, #13063, #53, #12838, #11902, #3566, #6914, #6074, #10758, #281, #4721, #2273 ),
 .UNSPECIFIED., .F., .F.,
 ( 4, 2, 2, 2, 2, 2, 2, 2, 2, 2, 4 ),
 ( 0.000000000000000000, 0.001575913261410275554, 0.002363869892115413440, 0.003151826522820551108, 0.004727739784230826879, 0.006303653045641103084, 0.007091609676346248559, 0.007879566307051392299, 0.009455479568461672840, 0.01103139282987195165, 0.01260730609128223219 ),
 .UNSPECIFIED. ) ;
#6249 = DIRECTION ( 'NONE',  ( -8.018662683283438208E-16, 5.975035461963189015E-16, 1.000000000000000000 ) ) ;
#6250 = VERTEX_POINT ( 'NONE', #15044 ) ;
#6251 = CARTESIAN_POINT ( 'NONE',  ( -14.45576569028314218, -52.45646407435158665, -17.98672605992057072 ) ) ;
#6252 = EDGE_CURVE ( 'NONE', #9932, #9450, #9454, .T. ) ;
#6253 = LINE ( 'NONE', #464, #6526 ) ;
#6254 = EDGE_CURVE ( 'NONE', #415, #2422, #6920, .T. ) ;
#6255 = ORIENTED_EDGE ( 'NONE', *, *, #14579, .F. ) ;
#6256 = DIRECTION ( 'NONE',  ( 8.018662683283438208E-16, -5.975035461963189015E-16, -1.000000000000000000 ) ) ;
#6257 = ORIENTED_EDGE ( 'NONE', *, *, #8260, .T. ) ;
#6259 = ORIENTED_EDGE ( 'NONE', *, *, #4819, .T. ) ;
#6258 = CARTESIAN_POINT ( 'NONE',  ( -36.51509609678214474, -37.41693849659213811, -11.55597063191085283 ) ) ;
#6260 = ORIENTED_EDGE ( 'NONE', *, *, #8377, .F. ) ;
#6261 = ADVANCED_BREP_SHAPE_REPRESENTATION ( '', ( #12764, #6789 ), #14627 ) ;
#6262 = DIRECTION ( 'NONE',  ( 0.9320450512859426162, 0.3618458327180910095, -0.01896353653557698513 ) ) ;
#6263 = VECTOR ( 'NONE', #2689, 999.9999999999998863 ) ;
#6264 = ORIENTED_EDGE ( 'NONE', *, *, #3004, .F. ) ;
#6265 = LINE ( 'NONE', #3985, #5729 ) ;
#6266 = PRESENTATION_LAYER_ASSIGNMENT (  '', '', ( #13611 ) ) ;
#6267 = PRODUCT_DEFINITION_SHAPE ( 'NONE', 'NONE',  #15132 ) ;
#6268 = LINE ( 'NONE', #11096, #10417 ) ;
#6269 = SHAPE_DEFINITION_REPRESENTATION ( #793, #3931 ) ;
#6270 = CIRCLE ( 'NONE', #12647, 2.499999999999998668 ) ;
#6271 = CARTESIAN_POINT ( 'NONE',  ( -15.49969986081099371, -32.00737899243799234, -13.28793577849899599 ) ) ;
#6272 = EDGE_CURVE ( 'NONE', #12486, #7429, #7067, .T. ) ;
#6273 = EDGE_CURVE ( 'NONE', #10559, #7319, #3420, .T. ) ;
#6274 = AXIS2_PLACEMENT_3D ( 'NONE', #12365, #8912, #4256 ) ;
#6275 = CARTESIAN_POINT ( 'NONE',  ( -7.504258367036227284, -44.23032460206619731, 45.54293165267414878 ) ) ;
#6276 = DIRECTION ( 'NONE',  ( 0.000000000000000000, 0.000000000000000000, 1.000000000000000000 ) ) ;
#6277 = ORIENTED_EDGE ( 'NONE', *, *, #4317, .T. ) ;
#6278 = CARTESIAN_POINT ( 'NONE',  ( -15.49969986081095996, -67.00737899243799234, -5.497689735156000346 ) ) ;
#6280 = VERTEX_POINT ( 'NONE', #6990 ) ;
#6279 = CARTESIAN_POINT ( 'NONE',  ( -23.54151295824578227, -12.77219731018227300, 56.85231026484398598 ) ) ;
#6281 = CIRCLE ( 'NONE', #3109, 0.4500000000000011768 ) ;
#6282 = ORIENTED_EDGE ( 'NONE', *, *, #3434, .T. ) ;
#6283 = DIRECTION ( 'NONE',  ( 0.5975035461963189576, 0.8018662683283437342, 0.000000000000000000 ) ) ;
#6284 = CARTESIAN_POINT ( 'NONE',  ( -15.61203582817000068, -107.8163049764641812, -5.262754992868533321 ) ) ;
#6285 = ORIENTED_EDGE ( 'NONE', *, *, #6831, .F. ) ;
#6286 = CARTESIAN_POINT ( 'NONE',  ( -21.48581293389291247, -5.528213918555015205, 57.00231026484397745 ) ) ;
#6287 = CIRCLE ( 'NONE', #14841, 9.974999999999999645 ) ;
#6288 = VECTOR ( 'NONE', #10825, 1000.000000000000000 ) ;
#6289 = EDGE_CURVE ( 'NONE', #1092, #1495, #6034, .T. ) ;
#6290 = CARTESIAN_POINT ( 'NONE',  ( -22.61924992783766797, -9.696439889920343447, 57.00231026484397745 ) ) ;
#6291 = CARTESIAN_POINT ( 'NONE',  ( -12.52039621090187893, -4.935039769003430443, 56.85231026484398598 ) ) ;
#6293 = CARTESIAN_POINT ( 'NONE',  ( -34.10648070438527668, 6.836425395143246320, 18.03001900748674657 ) ) ;
#6292 = DIRECTION ( 'NONE',  ( -0.9755678736739584744, 0.2196982563774038943, -9.135454576426008610E-16 ) ) ;
#6294 = EDGE_LOOP ( 'NONE', ( #14572, #8163, #10345, #2664 ) ) ;
#6295 = LINE ( 'NONE', #4163, #12662 ) ;
#6296 = CARTESIAN_POINT ( 'NONE',  ( -15.49969986081092266, -109.4443699603185109, -0.1262635860074601546 ) ) ;
#6297 = ORIENTED_EDGE ( 'NONE', *, *, #7383, .F. ) ;
#6298 = ORIENTED_EDGE ( 'NONE', *, *, #15072, .F. ) ;
#6299 = CARTESIAN_POINT ( 'NONE',  ( -23.24400209454358901, -46.58079323946816430, 56.19408944517149962 ) ) ;
#6300 = VERTEX_POINT ( 'NONE', #4880 ) ;
#6301 = DIRECTION ( 'NONE',  ( 0.9931883319083342210, -0.1165201156931306992, 0.000000000000000000 ) ) ;
#6302 = CIRCLE ( 'NONE', #9494, 9.974999999999999645 ) ;
#6303 = ADVANCED_FACE ( 'NONE', ( #14203 ), #12684, .F. ) ;
#6304 = CARTESIAN_POINT ( 'NONE',  ( -7.490307934913750465, -12.48011759562962020, 57.00231026484399166 ) ) ;
#6305 = CARTESIAN_POINT ( 'NONE',  ( -20.68283285135230898, -106.4450808729558560, -6.911160851980194586 ) ) ;
#6306 = CARTESIAN_POINT ( 'NONE',  ( -8.489236575244433425, -20.67953079448830422, 56.34577682959393741 ) ) ;
#6307 = CARTESIAN_POINT ( 'NONE',  ( -20.61203582816999713, -107.1622034095870077, -6.087689735156005533 ) ) ;
#6308 = DIRECTION ( 'NONE',  ( 8.018662683283438208E-16, -5.975035461963189015E-16, -1.000000000000000000 ) ) ;
#6309 = EDGE_LOOP ( 'NONE', ( #9981, #10442, #5061, #13266 ) ) ;
#6310 = CARTESIAN_POINT ( 'NONE',  ( -18.18846581869429713, -17.11577719991581148, -13.99768973515600301 ) ) ;
#6311 = DIRECTION ( 'NONE',  ( -8.018662683283438208E-16, 5.975035461963189015E-16, 1.000000000000000000 ) ) ;
#6312 = ORIENTED_EDGE ( 'NONE', *, *, #12158, .F. ) ;
#6313 = CARTESIAN_POINT ( 'NONE',  ( 22.00029349158540626, -23.75745569556128345, 24.42532365904204283 ) ) ;
#6314 = CARTESIAN_POINT ( 'NONE',  ( -15.45378054160984682, -13.48759475315262613, 56.85231026484398598 ) ) ;
#6315 = ORIENTED_EDGE ( 'NONE', *, *, #8192, .F. ) ;
#6316 = FACE_OUTER_BOUND ( 'NONE', #10947, .T. ) ;
#6317 = EDGE_LOOP ( 'NONE', ( #4616, #3145, #9353, #3499 ) ) ;
#6318 = CARTESIAN_POINT ( 'NONE',  ( -15.49969986081091733, -13.50737899243822682, 54.00231026484399166 ) ) ;
#6319 = CLOSED_SHELL ( 'NONE', ( #12229, #6986, #880, #10763, #1591, #5316, #5618, #2343, #7205, #4748, #8844, #7972, #9455, #12992 ) ) ;
#6320 = EDGE_CURVE ( 'NONE', #9709, #6890, #12990, .T. ) ;
#6321 = DIRECTION ( 'NONE',  ( 0.5975035461963189576, 0.8018662683283437342, 0.000000000000000000 ) ) ;
#6322 = AXIS2_PLACEMENT_3D ( 'NONE', #627, #8654, #9949 ) ;
#6323 = VECTOR ( 'NONE', #9384, 1000.000000000000000 ) ;
#6324 = ADVANCED_FACE ( 'NONE', ( #3723 ), #2279, .F. ) ;
#6325 = DIRECTION ( 'NONE',  ( 0.000000000000000000, 0.000000000000000000, 1.000000000000000000 ) ) ;
#6326 = CARTESIAN_POINT ( 'NONE',  ( 16.20074900174340726, -30.09470171131693661, 4.177619646552957811 ) ) ;
#6327 = DIRECTION ( 'NONE',  ( -8.018662683283438208E-16, 5.975035461963189015E-16, 1.000000000000000000 ) ) ;
#6328 = ORIENTED_EDGE ( 'NONE', *, *, #11666, .T. ) ;
#6329 = CARTESIAN_POINT ( 'NONE',  ( -32.97257072231203523, 8.982922429331180680, 31.67529590550448404 ) ) ;
#6330 =( BOUNDED_CURVE ( )  B_SPLINE_CURVE ( 3, ( #1555, #5004, #10965, #3845 ),
 .UNSPECIFIED., .F., .T. ) 
 B_SPLINE_CURVE_WITH_KNOTS ( ( 4, 4 ),
 ( 0.7562501201432320075, 1.227990006496096020 ),
 .UNSPECIFIED. ) 
 CURVE ( )  GEOMETRIC_REPRESENTATION_ITEM ( )  RATIONAL_B_SPLINE_CURVE ( ( 1.000000000000000000, 0.9815409421278752378, 0.9815409421278752378, 1.000000000000000000 ) ) 
 REPRESENTATION_ITEM ( '' )  );
#6331 = LINE ( 'NONE', #2898, #3368 ) ;
#6332 = ORIENTED_EDGE ( 'NONE', *, *, #9174, .T. ) ;
#6333 = ORIENTED_EDGE ( 'NONE', *, *, #7932, .F. ) ;
#6335 = ORIENTED_EDGE ( 'NONE', *, *, #2986, .F. ) ;
#6334 = CARTESIAN_POINT ( 'NONE',  ( 2.500300139188998738, -46.50737899243799944, 47.00231026484399877 ) ) ;
#6336 = ORIENTED_EDGE ( 'NONE', *, *, #1315, .F. ) ;
#6337 = CIRCLE ( 'NONE', #8786, 9.974999999999999645 ) ;
#6338 = DIRECTION ( 'NONE',  ( 0.5779813897169902015, -0.8160499452489515804, 9.510565162951535624E-16 ) ) ;
#6339 = ORIENTED_EDGE ( 'NONE', *, *, #13296, .F. ) ;
#6340 = EDGE_CURVE ( 'NONE', #5098, #12074, #12402, .T. ) ;
#6341 = EDGE_CURVE ( 'NONE', #8351, #1553, #2395, .T. ) ;
#6342 = CARTESIAN_POINT ( 'NONE',  ( -33.30392703919734743, 7.441414002149839391, 17.57488669123580749 ) ) ;
#6343 = EDGE_CURVE ( 'NONE', #10539, #2418, #4648, .T. ) ;
#6344 = LINE ( 'NONE', #2766, #8064 ) ;
#6345 = CARTESIAN_POINT ( 'NONE',  ( -21.24026693782044717, -7.828337292084670551, 56.85231026484398598 ) ) ;
#6346 = EDGE_CURVE ( 'NONE', #1229, #6874, #6376, .T. ) ;
#6347 = PLANE ( 'NONE',  #14245 ) ;
#6348 = VERTEX_POINT ( 'NONE', #12210 ) ;
#6349 = LINE ( 'NONE', #1620, #1747 ) ;
#6350 = EDGE_LOOP ( 'NONE', ( #4105, #6365, #1381, #10719 ) ) ;
#6351 = DIRECTION ( 'NONE',  ( -1.000000000000000078E-15, 1.000000000000000000, 0.000000000000000000 ) ) ;
#6352 = ORIENTED_EDGE ( 'NONE', *, *, #13124, .F. ) ;
#6353 = VERTEX_POINT ( 'NONE', #11906 ) ;
#6354 = FACE_OUTER_BOUND ( 'NONE', #11425, .T. ) ;
#6355 = ORIENTED_EDGE ( 'NONE', *, *, #12044, .T. ) ;
#6356 = CARTESIAN_POINT ( 'NONE',  ( -8.663330333365388825, -17.80566954616001496, 57.00231026484399166 ) ) ;
#6357 = EDGE_CURVE ( 'NONE', #11198, #12259, #369, .T. ) ;
#6358 = DIRECTION ( 'NONE',  ( -0.5779813897169993053, 0.8160499452489450301, -9.510565162951571123E-16 ) ) ;
#6359 = DIRECTION ( 'NONE',  ( 0.000000000000000000, -2.168404344971008868E-16, 1.000000000000000000 ) ) ;
#6361 = DIRECTION ( 'NONE',  ( -8.018662683283438208E-16, 5.975035461963189015E-16, 1.000000000000000000 ) ) ;
#6360 = CARTESIAN_POINT ( 'NONE',  ( -24.33650094517379614, -11.44044972528773130, 56.85231026484398598 ) ) ;
#6362 = ORIENTED_EDGE ( 'NONE', *, *, #14575, .F. ) ;
#6363 = DIRECTION ( 'NONE',  ( 1.000000000000000000, 0.000000000000000000, 0.000000000000000000 ) ) ;
#6364 = DIRECTION ( 'NONE',  ( 0.5975035461963189576, 0.8018662683283437342, 0.000000000000000000 ) ) ;
#6365 = ORIENTED_EDGE ( 'NONE', *, *, #12435, .F. ) ;
#6366 = ORIENTED_EDGE ( 'NONE', *, *, #5057, .T. ) ;
#6367 = VECTOR ( 'NONE', #13425, 1000.000000000000000 ) ;
#6368 = EDGE_CURVE ( 'NONE', #1908, #1644, #5102, .T. ) ;
#6369 = DIRECTION ( 'NONE',  ( 0.000000000000000000, 0.1872998510044983078, 0.9823027872370578839 ) ) ;
#6370 = ORIENTED_EDGE ( 'NONE', *, *, #11309, .F. ) ;
#6371 = LINE ( 'NONE', #1646, #12785 ) ;
#6372 = CARTESIAN_POINT ( 'NONE',  ( 9.000300139189000959, -27.00737899243800300, 40.71206422150099513 ) ) ;
#6373 = FACE_OUTER_BOUND ( 'NONE', #9379, .T. ) ;
#6374 = CIRCLE ( 'NONE', #12760, 9.974999999999999645 ) ;
#6375 = DIRECTION ( 'NONE',  ( -8.018662683283438208E-16, 5.975035461963189015E-16, 1.000000000000000000 ) ) ;
#6376 = B_SPLINE_CURVE_WITH_KNOTS ( 'NONE', 3,
 ( #2355, #11675, #5851, #10529, #2803, #10985, #10837, #1651, #12132, #1505, #9839, #8610, #13362, #9686, #14359, #14578, #7532, #7305, #13297, #437, #7455, #3798, #5027, #2578, #5248, #11987, #10909, #6306, #3874, #1431 ),
 .UNSPECIFIED., .F., .F.,
 ( 4, 2, 2, 2, 1, 1, 1, 1, 2, 2, 2, 2, 2, 1, 1, 2, 2, 4 ),
 ( 0.000000000000000000, 0.2500000000000077161, 0.3750000000000112688, 0.4375000000000130451, 0.4687500000000140443, 0.4843750000000142664, 0.4921875000000144329, 0.4960937500000142664, 0.4980468750000140443, 0.5000000000000137668, 0.6250000000000028866, 0.6874999999999971134, 0.7187499999999943379, 0.7343749999999925615, 0.7421874999999923395, 0.7460937499999922284, 0.7499999999999921174, 1.000000000000000000 ),
 .UNSPECIFIED. ) ;
#6377 = DIRECTION ( 'NONE',  ( 0.000000000000000000, 1.000000000000000000, 0.000000000000000000 ) ) ;
#6378 = LINE ( 'NONE', #10128, #11811 ) ;
#6379 = ORIENTED_EDGE ( 'NONE', *, *, #9908, .T. ) ;
#6380 = PLANE ( 'NONE',  #4090 ) ;
#6381 = CARTESIAN_POINT ( 'NONE',  ( -19.62128088291994388, -20.45131122700032833, 56.85231026484398598 ) ) ;
#6382 = EDGE_CURVE ( 'NONE', #3863, #4618, #5281, .T. ) ;
#6383 = ORIENTED_EDGE ( 'NONE', *, *, #4928, .T. ) ;
#6384 = EDGE_CURVE ( 'NONE', #4372, #5367, #5167, .T. ) ;
#6385 = AXIS2_PLACEMENT_3D ( 'NONE', #3320, #5758, #3250 ) ;
#6386 = CARTESIAN_POINT ( 'NONE',  ( -23.54764701038621411, -12.84694604531765272, 57.00231026484397745 ) ) ;
#6387 = DIRECTION ( 'NONE',  ( 0.000000000000000000, 1.131341397376178572E-16, -1.000000000000000000 ) ) ;
#6388 = ORIENTED_EDGE ( 'NONE', *, *, #13359, .F. ) ;
#6389 = LINE ( 'NONE', #12373, #4739 ) ;
#6390 = ORIENTED_EDGE ( 'NONE', *, *, #6675, .T. ) ;
#6391 = AXIS2_PLACEMENT_3D ( 'NONE', #13172, #4338, #7249 ) ;
#6392 = PRODUCT_DEFINITION_SHAPE ( 'NONE', 'NONE',  #15131 ) ;
#6393 = AXIS2_PLACEMENT_3D ( 'NONE', #11169, #1988, #5353 ) ;
#6394 = DIRECTION ( 'NONE',  ( 0.000000000000000000, -2.185478394931410082E-16, 1.000000000000000000 ) ) ;
#6395 = CARTESIAN_POINT ( 'NONE',  ( -7.500433020662215178, -49.00523987278725713, 19.39053537552759821 ) ) ;
#6396 = AXIS2_PLACEMENT_3D ( 'NONE', #12206, #12431, #7236 ) ;
#6397 = CIRCLE ( 'NONE', #9800, 9.974999999999999645 ) ;
#6398 = AXIS2_PLACEMENT_3D ( 'NONE', #11719, #4766, #14253 ) ;
#6399 = CARTESIAN_POINT ( 'NONE',  ( -9.565488148413143321, -20.37370125056455095, 56.85231026484400019 ) ) ;
#6400 = PLANE ( 'NONE',  #6211 ) ;
#6401 = VERTEX_POINT ( 'NONE', #584 ) ;
#6402 = CARTESIAN_POINT ( 'NONE',  ( -15.49969986081092088, -13.50737899243822504, 56.85231026484398598 ) ) ;
#6403 = CARTESIAN_POINT ( 'NONE',  ( -7.501944906337848273, -44.50613385756380325, -4.001965388595783324 ) ) ;
#6404 = EDGE_CURVE ( 'NONE', #3050, #8123, #3117, .T. ) ;
#6405 = ORIENTED_EDGE ( 'NONE', *, *, #7655, .F. ) ;
#6406 = ORIENTED_EDGE ( 'NONE', *, *, #3749, .F. ) ;
#6408 = ORIENTED_EDGE ( 'NONE', *, *, #14044, .F. ) ;
#6407 = CARTESIAN_POINT ( 'NONE',  ( -35.39631831511088222, -38.07367433585212524, -12.28530471890510434 ) ) ;
#6409 = ORIENTED_EDGE ( 'NONE', *, *, #15036, .F. ) ;
#6410 = DIRECTION ( 'NONE',  ( 0.000000000000000000, 0.1872998510044689147, 0.9823027872370635460 ) ) ;
#6411 = LINE ( 'NONE', #11092, #1176 ) ;
#6412 = CONICAL_SURFACE ( 'NONE', #7881, 4.499999999999999112, 0.7853981633974476129 ) ;
#6413 = B_SPLINE_CURVE_WITH_KNOTS ( 'NONE', 3,
 ( #6094, #3741, #4815, #1592 ),
 .UNSPECIFIED., .F., .F.,
 ( 4, 4 ),
 ( 0.01169941957287599921, 0.01381006638855979997 ),
 .UNSPECIFIED. ) ;
#6414 = CARTESIAN_POINT ( 'NONE',  ( -15.49969986081099727, -107.2547982693967583, -7.854504911766861497 ) ) ;
#6415 = DIRECTION ( 'NONE',  ( -1.000000000000000000, -1.201369187114119994E-15, -9.616040805000176517E-16 ) ) ;
#6416 = DIRECTION ( 'NONE',  ( -1.000000000000000000, 1.291538348938060198E-32, -1.054621095516909827E-16 ) ) ;
#6417 = LINE ( 'NONE', #1841, #1177 ) ;
#6418 = DIRECTION ( 'NONE',  ( 1.000000000000000000, -1.291538348938060198E-32, 1.054621095516909827E-16 ) ) ;
#6419 = AXIS2_PLACEMENT_3D ( 'NONE', #10390, #9009, #3354 ) ;
#6420 = CARTESIAN_POINT ( 'NONE',  ( -7.480766807389218620, -12.55450823271226746, 56.85231026484400019 ) ) ;
#6421 = ADVANCED_FACE ( 'NONE', ( #8378 ), #13068, .F. ) ;
#6422 = ORIENTED_EDGE ( 'NONE', *, *, #13277, .F. ) ;
#6423 = AXIS2_PLACEMENT_3D ( 'NONE', #12668, #15028, #15103 ) ;
#6424 = ORIENTED_EDGE ( 'NONE', *, *, #10546, .F. ) ;
#6425 = CARTESIAN_POINT ( 'NONE',  ( -15.49969986081099194, -110.1520963948262732, -11.15368910512049894 ) ) ;
#6427 = VERTEX_POINT ( 'NONE', #13220 ) ;
#6426 = CARTESIAN_POINT ( 'NONE',  ( -7.497874475122997318, -44.50608669435617770, -6.993290823733421036 ) ) ;
#6428 = VERTEX_POINT ( 'NONE', #4953 ) ;
#6429 = EDGE_CURVE ( 'NONE', #7470, #3379, #9609, .T. ) ;
#6430 = DIRECTION ( 'NONE',  ( 0.000000000000000000, 1.850371707708594316E-16, -1.000000000000000000 ) ) ;
#6432 = ORIENTED_EDGE ( 'NONE', *, *, #12455, .T. ) ;
#6431 = LINE ( 'NONE', #14629, #13541 ) ;
#6433 = CARTESIAN_POINT ( 'NONE',  ( -12.10927446591014700, -10.53397642412856072, -13.13493504121917432 ) ) ;
#6434 = EDGE_CURVE ( 'NONE', #8805, #10153, #7256, .T. ) ;
#6435 = CIRCLE ( 'NONE', #8649, 9.974999999999999645 ) ;
#6436 = PLANE ( 'NONE',  #4414 ) ;
#6437 = CARTESIAN_POINT ( 'NONE',  ( -15.49969986081099904, 4.873818854045000037, 24.21206422150099868 ) ) ;
#6439 = FACE_OUTER_BOUND ( 'NONE', #10620, .T. ) ;
#6438 = CARTESIAN_POINT ( 'NONE',  ( -23.14528701667493849, -16.10665716956490812, 56.85231026484398598 ) ) ;
#6440 = EDGE_CURVE ( 'NONE', #2941, #9718, #2724, .T. ) ;
#6441 = ORIENTED_EDGE ( 'NONE', *, *, #4767, .T. ) ;
#6442 = CARTESIAN_POINT ( 'NONE',  ( -18.09969986081099336, -110.0345591146135860, -9.886379190557276431 ) ) ;
#6443 = EDGE_CURVE ( 'NONE', #8706, #2715, #9213, .T. ) ;
#6444 = CARTESIAN_POINT ( 'NONE',  ( -18.09969986081091875, -107.1622034095862972, -5.012689735156002691 ) ) ;
#6445 = ORIENTED_EDGE ( 'NONE', *, *, #11168, .T. ) ;
#6446 = VERTEX_POINT ( 'NONE', #7819 ) ;
#6447 = VECTOR ( 'NONE', #3573, 999.9999999999998863 ) ;
#6448 = CARTESIAN_POINT ( 'NONE',  ( -20.38837171516173186, -50.86174603611942757, 56.68489931584038288 ) ) ;
#6449 = ORIENTED_EDGE ( 'NONE', *, *, #3300, .T. ) ;
#6450 = CARTESIAN_POINT ( 'NONE',  ( -15.49969986081099904, -36.50737899243799944, 57.00231026484399877 ) ) ;
#6451 = CARTESIAN_POINT ( 'NONE',  ( 4.484189283470824350, 6.179576214047821203, 18.66823039591405120 ) ) ;
#6452 = DIRECTION ( 'NONE',  ( 0.1165201156931293391, 0.9931883319083343320, -4.999999999999998416E-16 ) ) ;
#6453 = AXIS2_PLACEMENT_3D ( 'NONE', #3742, #651, #13294 ) ;
#6454 = CARTESIAN_POINT ( 'NONE',  ( -15.50552586659557797, -13.55703840903364288, 56.85231026484398598 ) ) ;
#6455 = DIRECTION ( 'NONE',  ( 1.000000000000000000, 0.000000000000000000, 0.000000000000000000 ) ) ;
#6456 = PLANE ( 'NONE',  #7403 ) ;
#6457 = VERTEX_POINT ( 'NONE', #1807 ) ;
#6458 = CARTESIAN_POINT ( 'NONE',  ( -28.78282149594069850, -31.14135358865360104, -10.85656391856669778 ) ) ;
#6459 = EDGE_CURVE ( 'NONE', #1750, #14475, #6596, .T. ) ;
#6460 = CARTESIAN_POINT ( 'NONE',  ( -15.31527533914055539, -21.58027268651140673, 56.85231026484400019 ) ) ;
#6461 = ORIENTED_EDGE ( 'NONE', *, *, #10640, .T. ) ;
#6462 = CARTESIAN_POINT ( 'NONE',  ( 21.88645104390297647, -25.56672272642999033, 21.29103469435690954 ) ) ;
#6463 = PLANE ( 'NONE',  #2293 ) ;
#6464 = ORIENTED_EDGE ( 'NONE', *, *, #14642, .T. ) ;
#6465 = LINE ( 'NONE', #12452, #2960 ) ;
#6466 = VECTOR ( 'NONE', #13102, 1000.000000000000000 ) ;
#6467 = CARTESIAN_POINT ( 'NONE',  ( -19.87664613915258371, -5.557310358991672139, 56.85231026484398598 ) ) ;
#6468 = ADVANCED_FACE ( 'NONE', ( #7680 ), #13442, .T. ) ;
#6469 = CARTESIAN_POINT ( 'NONE',  ( -7.821737630532772378, -18.34578224045527151, 57.00231026484399166 ) ) ;
#6470 = CARTESIAN_POINT ( 'NONE',  ( -9.204203523554131294, -8.449911655164932256, 57.00231026484397745 ) ) ;
#6471 = LINE ( 'NONE', #13607, #10360 ) ;
#6472 = ORIENTED_EDGE ( 'NONE', *, *, #7482, .T. ) ;
#6473 = CARTESIAN_POINT ( 'NONE',  ( -32.76014075162859740, 10.68321993080349763, 32.15417856559049881 ) ) ;
#6474 = VECTOR ( 'NONE', #2124, 1000.000000000000000 ) ;
#6475 = CARTESIAN_POINT ( 'NONE',  ( -7.742611511953769288, -46.45389122984595076, -2.997689585474093477 ) ) ;
#6476 = VERTEX_POINT ( 'NONE', #8977 ) ;
#6478 = VERTEX_POINT ( 'NONE', #5538 ) ;
#6477 = CARTESIAN_POINT ( 'NONE',  ( -37.90618493125413124, -37.00737899243799234, -10.57698671581674077 ) ) ;
#6479 = ORIENTED_EDGE ( 'NONE', *, *, #9342, .F. ) ;
#6480 = DIRECTION ( 'NONE',  ( -8.018662683283438208E-16, 5.975035461963189015E-16, 1.000000000000000000 ) ) ;
#6481 = CARTESIAN_POINT ( 'NONE',  ( -17.54761070396351741, -21.31837676343380750, 57.00231026484399166 ) ) ;
#6482 = CARTESIAN_POINT ( 'NONE',  ( -18.36422177163696290, -5.957162821864243618, 56.85231026484398598 ) ) ;
#6483 = CYLINDRICAL_SURFACE ( 'NONE', #12090, 9.974999999999997868 ) ;
#6484 = VECTOR ( 'NONE', #14992, 1000.000000000000000 ) ;
#6485 = EDGE_CURVE ( 'NONE', #6873, #9624, #12436, .T. ) ;
#6486 = CARTESIAN_POINT ( 'NONE',  ( -28.40830458780451551, -109.6305988279009966, -3.679722063549803135 ) ) ;
#6487 = CARTESIAN_POINT ( 'NONE',  ( -18.09969986081092586, -95.91433005893298969, -10.19792577984107318 ) ) ;
#6488 = DIRECTION ( 'NONE',  ( 0.000000000000000000, 0.000000000000000000, -1.000000000000000000 ) ) ;
#6489 = CARTESIAN_POINT ( 'NONE',  ( -15.42469993581076970, -23.50709773904532085, 57.00223526491900117 ) ) ;
#6490 = CARTESIAN_POINT ( 'NONE',  ( 13.85920135429429934, -27.00737899243800300, 26.71206422150099868 ) ) ;
#6491 = EDGE_LOOP ( 'NONE', ( #1149, #1947, #8335, #5565 ) ) ;
#6492 = FACE_OUTER_BOUND ( 'NONE', #12601, .T. ) ;
#6493 = AXIS2_PLACEMENT_3D ( 'NONE', #81, #11850, #3670 ) ;
#6494 = ORIENTED_EDGE ( 'NONE', *, *, #5114, .F. ) ;
#6495 = CARTESIAN_POINT ( 'NONE',  ( 4.000300139189000959, -19.50737899243798879, -17.99768973515599768 ) ) ;
#6497 = ORIENTED_EDGE ( 'NONE', *, *, #13423, .F. ) ;
#6496 = LINE ( 'NONE', #7504, #14973 ) ;
#6498 = ORIENTED_EDGE ( 'NONE', *, *, #9633, .F. ) ;
#6499 = CARTESIAN_POINT ( 'NONE',  ( -13.08902965115471417, -15.30366854329086834, 57.00231026484398456 ) ) ;
#6501 = ORIENTED_EDGE ( 'NONE', *, *, #7464, .T. ) ;
#6500 = CARTESIAN_POINT ( 'NONE',  ( 1.785016747259931202, 10.36523356804368845, 16.32270781623988753 ) ) ;
#6502 = AXIS2_PLACEMENT_3D ( 'NONE', #7118, #13192, #3695 ) ;
#6503 = CARTESIAN_POINT ( 'NONE',  ( -15.49969986081099371, -9.007378992438001220, -13.28793577849899599 ) ) ;
#6504 = EDGE_CURVE ( 'NONE', #12569, #4606, #1881, .T. ) ;
#6505 = CARTESIAN_POINT ( 'NONE',  ( -15.61203582817000068, -106.5081018427098201, -6.912624477443467974 ) ) ;
#6506 = CARTESIAN_POINT ( 'NONE',  ( -10.07958688850791162, -7.521259601090221736, 56.85231026484398598 ) ) ;
#6507 = AXIS2_PLACEMENT_3D ( 'NONE', #750, #5338, #901 ) ;
#6508 = ADVANCED_FACE ( 'NONE', ( #7902 ), #12508, .F. ) ;
#6509 = CARTESIAN_POINT ( 'NONE',  ( -7.753733168396170328, -46.50737899243799944, 47.00231026484399877 ) ) ;
#6510 = AXIS2_PLACEMENT_3D ( 'NONE', #2072, #6418, #10091 ) ;
#6511 = CARTESIAN_POINT ( 'NONE',  ( -12.98295438134161195, -5.834228258119843247, 56.85231026484398598 ) ) ;
#6512 = VERTEX_POINT ( 'NONE', #11137 ) ;
#6513 = LINE ( 'NONE', #12197, #10454 ) ;
#6514 = LINE ( 'NONE', #14719, #157 ) ;
#6515 = VERTEX_POINT ( 'NONE', #7608 ) ;
#6516 = ORIENTED_EDGE ( 'NONE', *, *, #11975, .T. ) ;
#6517 = CARTESIAN_POINT ( 'NONE',  ( -15.61203582816999891, -106.7406604375499626, -7.297873098422156701 ) ) ;
#6518 = ORIENTED_EDGE ( 'NONE', *, *, #5564, .F. ) ;
#6519 = LINE ( 'NONE', #1719, #1291 ) ;
#6520 = AXIS2_PLACEMENT_3D ( 'NONE', #2999, #8881, #4227 ) ;
#6521 = EDGE_CURVE ( 'NONE', #10220, #8595, #14954, .T. ) ;
#6522 = DIRECTION ( 'NONE',  ( 1.000000000000000000, 1.000000000000000078E-15, 0.000000000000000000 ) ) ;
#6523 = CARTESIAN_POINT ( 'NONE',  ( -20.62737807198738693, -106.7814035276991120, -7.097650603566109773 ) ) ;
#6524 = EDGE_CURVE ( 'NONE', #10845, #13725, #5389, .T. ) ;
#6525 = CARTESIAN_POINT ( 'NONE',  ( -9.989347722329672052, -48.50737899243800655, -5.497689735156000346 ) ) ;
#6526 = VECTOR ( 'NONE', #9787, 1000.000000000000000 ) ;
#6527 = VECTOR ( 'NONE', #13646, 1000.000000000000000 ) ;
#6528 = DIRECTION ( 'NONE',  ( 1.000000000000000000, -1.499759782661860071E-32, 1.224646799147350002E-16 ) ) ;
#6529 = LINE ( 'NONE', #12510, #5215 ) ;
#6530 = AXIS2_PLACEMENT_3D ( 'NONE', #2032, #11364, #6905 ) ;
#6531 = AXIS2_PLACEMENT_3D ( 'NONE', #7423, #8570, #405 ) ;
#6532 = EDGE_LOOP ( 'NONE', ( #7430, #13504, #9116, #1329 ) ) ;
#6533 = LINE ( 'NONE', #8760, #1158 ) ;
#6534 = DIRECTION ( 'NONE',  ( 0.000000000000000000, 0.000000000000000000, 1.000000000000000000 ) ) ;
#6535 = ORIENTED_EDGE ( 'NONE', *, *, #4328, .T. ) ;
#6536 = EDGE_CURVE ( 'NONE', #11708, #11163, #8754, .T. ) ;
#6537 = CARTESIAN_POINT ( 'NONE',  ( -31.79969986081099975, 11.99262100756199878, 32.26206422150099939 ) ) ;
#6538 = CARTESIAN_POINT ( 'NONE',  ( 21.98614235536664197, -23.92397303140615605, 25.26083157490126752 ) ) ;
#6539 = DIRECTION ( 'NONE',  ( -0.9437508163134049610, -0.3306575217771128283, -5.591929034707468788E-16 ) ) ;
#6540 = VERTEX_POINT ( 'NONE', #655 ) ;
#6541 = LINE ( 'NONE', #746, #13712 ) ;
#6542 = B_SPLINE_CURVE_WITH_KNOTS ( 'NONE', 3,
 ( #4609, #8187, #98, #2612, #9263, #5887 ),
 .UNSPECIFIED., .F., .F.,
 ( 4, 2, 4 ),
 ( 0.002335154401881610765, 0.002868089949059464579, 0.003401025496237318393 ),
 .UNSPECIFIED. ) ;
#6543 = CYLINDRICAL_SURFACE ( 'NONE', #13918, 3.250000000000002665 ) ;
#6544 = EDGE_CURVE ( 'NONE', #2885, #6427, #13587, .T. ) ;
#6545 = EDGE_CURVE ( 'NONE', #3162, #4803, #14880, .T. ) ;
#6546 = APPLICATION_PROTOCOL_DEFINITION ( 'draft international standard', 'automotive_design', 1998, #4007 ) ;
#6547 = FACE_OUTER_BOUND ( 'NONE', #9414, .T. ) ;
#6548 =( BOUNDED_CURVE ( )  B_SPLINE_CURVE ( 3, ( #14807, #14885, #11366, #13814 ),
 .UNSPECIFIED., .F., .F. ) 
 B_SPLINE_CURVE_WITH_KNOTS ( ( 4, 4 ),
 ( 5.024656459356720006, 6.283185307179586232 ),
 .UNSPECIFIED. ) 
 CURVE ( )  GEOMETRIC_REPRESENTATION_ITEM ( )  RATIONAL_B_SPLINE_CURVE ( ( 1.000000000000000000, 0.8723071003127500500, 0.8723071003127500500, 1.000000000000000000 ) ) 
 REPRESENTATION_ITEM ( '' )  );
#6549 = DIRECTION ( 'NONE',  ( -1.000000000000000000, -1.201369187114119994E-15, -9.616040805000176517E-16 ) ) ;
#6550 = LINE ( 'NONE', #10072, #6932 ) ;
#6551 = VERTEX_POINT ( 'NONE', #10125 ) ;
#6552 = CARTESIAN_POINT ( 'NONE',  ( -32.78441646887873873, 10.36523356808538665, 32.10142062676905539 ) ) ;
#6553 = CARTESIAN_POINT ( 'NONE',  ( -31.79969986081099975, 20.99262100756200056, 32.26206422150099939 ) ) ;
#6554 = EDGE_LOOP ( 'NONE', ( #2053, #15105, #10332, #4295 ) ) ;
#6556 = ORIENTED_EDGE ( 'NONE', *, *, #9969, .F. ) ;
#6555 = DIRECTION ( 'NONE',  ( -0.7737441449604661736, -0.6334982226805353500, -2.419218955996689845E-16 ) ) ;
#6557 = ORIENTED_EDGE ( 'NONE', *, *, #2517, .F. ) ;
#6558 = EDGE_CURVE ( 'NONE', #2908, #14123, #5319, .T. ) ;
#6559 = CARTESIAN_POINT ( 'NONE',  ( -15.49969986081099016, -52.50737899243799944, 27.50231026484399521 ) ) ;
#6560 = CARTESIAN_POINT ( 'NONE',  ( -9.141872392333175057, -49.39150629834951900, 56.46061503045971364 ) ) ;
#6561 = AXIS2_PLACEMENT_3D ( 'NONE', #3842, #8726, #8505 ) ;
#6562 = LINE ( 'NONE', #12320, #8843 ) ;
#6563 = CARTESIAN_POINT ( 'NONE',  ( -8.492287438043703673, -48.36911050528196654, 42.82612708017594372 ) ) ;
#6564 = CARTESIAN_POINT ( 'NONE',  ( -16.49725497239786165, -3.582384846377125509, 54.00231026484397745 ) ) ;
#6565 = CARTESIAN_POINT ( 'NONE',  ( -15.49969986081099371, -57.00737899243799944, -17.99768973515599768 ) ) ;
#6566 = DIRECTION ( 'NONE',  ( -8.018662683283438208E-16, 5.975035461963189015E-16, 1.000000000000000000 ) ) ;
#6567 = CIRCLE ( 'NONE', #231, 37.50000000000000000 ) ;
#6568 = CARTESIAN_POINT ( 'NONE',  ( -7.512147529361665299, -44.06076409293740426, 45.03331134192608687 ) ) ;
#6569 = ORIENTED_EDGE ( 'NONE', *, *, #12893, .F. ) ;
#6570 = LINE ( 'NONE', #7868, #11032 ) ;
#6571 = EDGE_LOOP ( 'NONE', ( #11707, #12033, #9712, #6362 ) ) ;
#6572 = ORIENTED_EDGE ( 'NONE', *, *, #14931, .T. ) ;
#6573 = ORIENTED_EDGE ( 'NONE', *, *, #4513, .F. ) ;
#6574 = EDGE_CURVE ( 'NONE', #2938, #13270, #2554, .T. ) ;
#6576 = ORIENTED_EDGE ( 'NONE', *, *, #8508, .T. ) ;
#6575 = DIRECTION ( 'NONE',  ( -8.018662683283438208E-16, 5.975035461963189015E-16, 1.000000000000000000 ) ) ;
#6577 = FACE_OUTER_BOUND ( 'NONE', #13173, .T. ) ;
#6578 = CARTESIAN_POINT ( 'NONE',  ( -3.508527451665001351, -44.77532818486911736, -5.497689735156003010 ) ) ;
#6579 = VECTOR ( 'NONE', #11581, 1000.000000000000000 ) ;
#6580 = CARTESIAN_POINT ( 'NONE',  ( -7.821533452792987617, -47.59505538333905150, -7.749013365421348887 ) ) ;
#6581 = CARTESIAN_POINT ( 'NONE',  ( -15.49969986081092088, -109.4789632527123047, -0.7863429266504098347 ) ) ;
#6582 = VERTEX_POINT ( 'NONE', #1238 ) ;
#6583 = CARTESIAN_POINT ( 'NONE',  ( -5.499699860811000818, -46.50737899243799944, 16.50231026484399877 ) ) ;
#6584 = VERTEX_POINT ( 'NONE', #6116 ) ;
#6585 = DIRECTION ( 'NONE',  ( 0.000000000000000000, 1.000000000000000000, 1.224646799147350002E-16 ) ) ;
#6586 = ORIENTED_EDGE ( 'NONE', *, *, #8553, .T. ) ;
#6587 = ORIENTED_EDGE ( 'NONE', *, *, #4770, .T. ) ;
#6588 = EDGE_CURVE ( 'NONE', #470, #36, #11715, .T. ) ;
#6589 = DIRECTION ( 'NONE',  ( 0.2872152572324145892, 0.9578660637129379207, -3.420201433256678811E-16 ) ) ;
#6590 = VERTEX_POINT ( 'NONE', #3689 ) ;
#6591 = LINE ( 'NONE', #13081, #3984 ) ;
#6592 = EDGE_CURVE ( 'NONE', #10291, #12780, #7317, .T. ) ;
#6593 = AXIS2_PLACEMENT_3D ( 'NONE', #5206, #12249, #11172 ) ;
#6594 = CARTESIAN_POINT ( 'NONE',  ( 3.105701218396447860, 6.837078596092822202, 18.02952760507402985 ) ) ;
#6595 = CARTESIAN_POINT ( 'NONE',  ( 0.8918609567539013128, -25.75737899243799944, -123.9247733198440073 ) ) ;
#6596 = LINE ( 'NONE', #6525, #7997 ) ;
#6597 = UNCERTAINTY_MEASURE_WITH_UNIT (LENGTH_MEASURE( 1.000000000000000082E-05 ), #9580, 'distance_accuracy_value', 'NONE');
#6598 = CARTESIAN_POINT ( 'NONE',  ( -15.14850084941412511, -4.438867027711355107, 56.85231026484398598 ) ) ;
#6600 = FACE_OUTER_BOUND ( 'NONE', #3484, .T. ) ;
#6599 = CARTESIAN_POINT ( 'NONE',  ( -15.53979317422733786, -13.47750381512840967, 56.85231026484398598 ) ) ;
#6601 = ADVANCED_BREP_SHAPE_REPRESENTATION ( '', ( #7285, #6789 ), #8995 ) ;
#6602 = ORIENTED_EDGE ( 'NONE', *, *, #9017, .T. ) ;
#6603 = DIRECTION ( 'NONE',  ( 0.000000000000000000, -9.130123557772668334E-17, 1.000000000000000000 ) ) ;
#6604 = DIRECTION ( 'NONE',  ( 0.6334982226805353500, -0.7737441449604661736, 9.702957262759961121E-16 ) ) ;
#6605 = VERTEX_POINT ( 'NONE', #12959 ) ;
#6606 = DIRECTION ( 'NONE',  ( -0.6519834208811540188, -0.7582332219680881780, -6.975647374412566582E-17 ) ) ;
#6607 = EDGE_CURVE ( 'NONE', #1579, #12952, #12226, .T. ) ;
#6608 = PLANE ( 'NONE',  #13742 ) ;
#6609 = DIRECTION ( 'NONE',  ( -1.000000000000000000, -1.201369187114119994E-15, -9.616040805000176517E-16 ) ) ;
#6610 = CARTESIAN_POINT ( 'NONE',  ( 9.000300139189000959, -27.00737899243800300, 24.21206422150099868 ) ) ;
#6611 = ORIENTED_EDGE ( 'NONE', *, *, #6967, .F. ) ;
#6612 = CARTESIAN_POINT ( 'NONE',  ( -15.49969986081099194, -27.00737899243800300, 19.50231026484399877 ) ) ;
#6613 = EDGE_CURVE ( 'NONE', #12009, #6962, #9573, .T. ) ;
#6614 = AXIS2_PLACEMENT_3D ( 'NONE', #826, #14896, #5482 ) ;
#6615 = DIRECTION ( 'NONE',  ( 0.000000000000000000, -1.000000000000000000, -1.224646799147350002E-16 ) ) ;
#6616 = ADVANCED_FACE ( 'NONE', ( #14250 ), #7111, .T. ) ;
#6617 = DIRECTION ( 'NONE',  ( 2.213357799158899581E-16, -0.3283718064428475802, -0.9445485465202205777 ) ) ;
#6618 = DIRECTION ( 'NONE',  ( 1.000000000000000000, 1.201369187114119994E-15, 9.616040805000176517E-16 ) ) ;
#6619 = CARTESIAN_POINT ( 'NONE',  ( -15.49969986081099904, 70.81438635534659909, 17.96206422150100579 ) ) ;
#6620 = CARTESIAN_POINT ( 'NONE',  ( -5.628190034013323739, -14.94052892857136428, 54.00231026484399166 ) ) ;
#6621 = VECTOR ( 'NONE', #7201, 1000.000000000000114 ) ;
#6622 = ORIENTED_EDGE ( 'NONE', *, *, #3624, .F. ) ;
#6623 = DIRECTION ( 'NONE',  ( 0.000000000000000000, 0.000000000000000000, 1.000000000000000000 ) ) ;
#6624 = CARTESIAN_POINT ( 'NONE',  ( -14.61203582816999891, -107.5495670694337207, -7.066625679870575105 ) ) ;
#6625 = AXIS2_PLACEMENT_3D ( 'NONE', #11858, #13023, #8178 ) ;
#6626 = EDGE_CURVE ( 'NONE', #6250, #560, #9225, .T. ) ;
#6627 = EDGE_CURVE ( 'NONE', #12770, #11960, #2542, .T. ) ;
#6628 = VERTEX_POINT ( 'NONE', #2394 ) ;
#6630 = ORIENTED_EDGE ( 'NONE', *, *, #8604, .F. ) ;
#6629 = CARTESIAN_POINT ( 'NONE',  ( 22.00030013918900096, -27.00737899243800300, 24.21206422150099868 ) ) ;
#6631 = VERTEX_POINT ( 'NONE', #7033 ) ;
#6632 = CARTESIAN_POINT ( 'NONE',  ( 13.85920135429429934, -27.00737899243800300, 24.21206422150099868 ) ) ;
#6633 = DIRECTION ( 'NONE',  ( 0.000000000000000000, -1.000000000000000000, -1.224646799147350002E-16 ) ) ;
#6634 = VECTOR ( 'NONE', #10830, 1000.000000000000000 ) ;
#6635 = DIRECTION ( 'NONE',  ( 8.018662683283438208E-16, -5.975035461963189015E-16, -1.000000000000000000 ) ) ;
#6636 = FACE_OUTER_BOUND ( 'NONE', #5171, .T. ) ;
#6637 = AXIS2_PLACEMENT_3D ( 'NONE', #4020, #8394, #4244 ) ;
#6638 = CIRCLE ( 'NONE', #9583, 9.974999999999999645 ) ;
#6639 = VECTOR ( 'NONE', #2911, 1000.000000000000000 ) ;
#6640 = CARTESIAN_POINT ( 'NONE',  ( -23.45327702811275827, -7.487309620431347845, 54.00231026484397745 ) ) ;
#6641 = CARTESIAN_POINT ( 'NONE',  ( -15.61203582816999713, -108.0739631064533484, -6.614055049357310700 ) ) ;
#6642 = LINE ( 'NONE', #11397, #6053 ) ;
#6643 = CYLINDRICAL_SURFACE ( 'NONE', #9606, 0.2000000000000012046 ) ;
#6644 = ORIENTED_EDGE ( 'NONE', *, *, #8424, .F. ) ;
#6645 = CYLINDRICAL_SURFACE ( 'NONE', #13972, 0.2500000000000007216 ) ;
#6646 = AXIS2_PLACEMENT_3D ( 'NONE', #4701, #190, #2477 ) ;
#6647 = ORIENTED_EDGE ( 'NONE', *, *, #3956, .T. ) ;
#6648 = DIRECTION ( 'NONE',  ( 1.000000000000000000, 1.201369187114119994E-15, 9.616040805000176517E-16 ) ) ;
#6650 = ORIENTED_EDGE ( 'NONE', *, *, #12432, .F. ) ;
#6649 = CARTESIAN_POINT ( 'NONE',  ( -18.09470815789902076, -3.848709554607572692, 61.62351371178731796 ) ) ;
#6651 = ORIENTED_EDGE ( 'NONE', *, *, #8676, .T. ) ;
#6652 = CONICAL_SURFACE ( 'NONE', #7133, 5.000000000000000000, 0.7853981633974476129 ) ;
#6653 = LINE ( 'NONE', #11336, #7007 ) ;
#6654 = ORIENTED_EDGE ( 'NONE', *, *, #960, .F. ) ;
#6655 = DIRECTION ( 'NONE',  ( 3.202566417187950042E-16, 1.224646799147350002E-16, -1.000000000000000000 ) ) ;
#6656 = LINE ( 'NONE', #11339, #2575 ) ;
#6657 = CARTESIAN_POINT ( 'NONE',  ( -15.49969986081099016, -36.50737899243799944, 27.50231026484399521 ) ) ;
#6658 = EDGE_CURVE ( 'NONE', #11757, #9677, #1390, .T. ) ;
#6659 = EDGE_CURVE ( 'NONE', #3870, #6300, #11194, .T. ) ;
#6660 = AXIS2_PLACEMENT_3D ( 'NONE', #14162, #2456, #9644 ) ;
#6661 = AXIS2_PLACEMENT_3D ( 'NONE', #6599, #8758, #2109 ) ;
#6662 = LINE ( 'NONE', #715, #2235 ) ;
#6663 = CARTESIAN_POINT ( 'NONE',  ( -32.87150473820536689, -24.05954647699559601, -13.82452877272130642 ) ) ;
#6664 = ORIENTED_EDGE ( 'NONE', *, *, #3365, .T. ) ;
#6665 = CARTESIAN_POINT ( 'NONE',  ( 15.96494998288805789, -24.06893396188195311, 44.61485892283481292 ) ) ;
#6666 = ORIENTED_EDGE ( 'NONE', *, *, #5048, .F. ) ;
#6667 = CARTESIAN_POINT ( 'NONE',  ( 2.500300139188996518, -46.50737899243799944, 44.50231026484399877 ) ) ;
#6668 = EDGE_LOOP ( 'NONE', ( #555, #8336, #6260, #12263 ) ) ;
#6669 = VERTEX_POINT ( 'NONE', #1544 ) ;
#6670 = CARTESIAN_POINT ( 'NONE',  ( 2.500300139188999182, -42.00737899243800655, 52.39987856403599409 ) ) ;
#6671 = ORIENTED_EDGE ( 'NONE', *, *, #9548, .F. ) ;
#6672 = DIRECTION ( 'NONE',  ( 1.000000000000000000, 1.000000000000000078E-15, 0.000000000000000000 ) ) ;
#6673 = AXIS2_PLACEMENT_3D ( 'NONE', #5479, #8992, #13745 ) ;
#6674 = DIRECTION ( 'NONE',  ( 0.8018662683283437342, -0.5975035461963188466, 9.999999999999996833E-16 ) ) ;
#6675 = EDGE_CURVE ( 'NONE', #10716, #2060, #4689, .T. ) ;
#6676 = CARTESIAN_POINT ( 'NONE',  ( 14.82649946315277312, -25.88651038688090367, 2.153413930940738297 ) ) ;
#6677 = AXIS2_PLACEMENT_3D ( 'NONE', #10646, #4765, #14019 ) ;
#6678 = CARTESIAN_POINT ( 'NONE',  ( -7.742536611909244471, -46.45380687591467250, 22.00231042132131165 ) ) ;
#6680 = CARTESIAN_POINT ( 'NONE',  ( 6.920290371738591517, 5.009117329185531986, 28.17596432838387699 ) ) ;
#6679 = PLANE ( 'NONE',  #9858 ) ;
#6681 = VERTEX_POINT ( 'NONE', #8720 ) ;
#6682 = CARTESIAN_POINT ( 'NONE',  ( -11.67714598312096008, -19.46131314156662384, 56.85231026484400019 ) ) ;
#6683 = CARTESIAN_POINT ( 'NONE',  ( -3.508527451664998686, -47.80641709811465745, -4.747689735156000346 ) ) ;
#6684 = ORIENTED_EDGE ( 'NONE', *, *, #14200, .F. ) ;
#6685 = EDGE_LOOP ( 'NONE', ( #6264, #630 ) ) ;
#6686 = CARTESIAN_POINT ( 'NONE',  ( -20.87112600995945755, -109.7258744763782943, -5.497689735156006563 ) ) ;
#6687 = LINE ( 'NONE', #15111, #7856 ) ;
#6688 = DIRECTION ( 'NONE',  ( 0.000000000000000000, 0.1872998510044689147, 0.9823027872370635460 ) ) ;
#6689 = LINE ( 'NONE', #5401, #14034 ) ;
#6690 = AXIS2_PLACEMENT_3D ( 'NONE', #7134, #14267, #12049 ) ;
#6691 = ORIENTED_EDGE ( 'NONE', *, *, #5810, .T. ) ;
#6692 = FACE_OUTER_BOUND ( 'NONE', #9846, .T. ) ;
#6693 = AXIS2_PLACEMENT_3D ( 'NONE', #4135, #8791, #10948 ) ;
#6694 = DIRECTION ( 'NONE',  ( 0.8018662683283437342, -0.5975035461963188466, 9.999999999999996833E-16 ) ) ;
#6695 =( NAMED_UNIT ( * ) SI_UNIT ( $, .STERADIAN. ) SOLID_ANGLE_UNIT ( ) );
#6696 = EDGE_CURVE ( 'NONE', #14421, #11355, #3867, .T. ) ;
#6697 = LINE ( 'NONE', #11377, #11640 ) ;
#6698 = DIRECTION ( 'NONE',  ( 0.2536112499260065323, 0.9673062255102924389, -3.746065934159220994E-16 ) ) ;
#6699 = LINE ( 'NONE', #10000, #1087 ) ;
#6700 = EDGE_CURVE ( 'NONE', #13514, #1579, #9941, .T. ) ;
#6701 = ORIENTED_EDGE ( 'NONE', *, *, #5854, .T. ) ;
#6702 = CARTESIAN_POINT ( 'NONE',  ( -11.53159268371330093, -90.86154151202431706, -1.876852786247884985 ) ) ;
#6703 = CARTESIAN_POINT ( 'NONE',  ( -20.18599136182625742, -52.50737899243802786, -13.49768973515603676 ) ) ;
#6704 = VERTEX_POINT ( 'NONE', #12324 ) ;
#6706 = ORIENTED_EDGE ( 'NONE', *, *, #1617, .T. ) ;
#6705 = DIRECTION ( 'NONE',  ( -1.000000000000000000, 0.000000000000000000, 0.000000000000000000 ) ) ;
#6707 = VERTEX_POINT ( 'NONE', #2767 ) ;
#6708 = PLANE ( 'NONE',  #7376 ) ;
#6709 = CARTESIAN_POINT ( 'NONE',  ( -10.21738681012386429, -50.52121012465195093, 56.62897346558520439 ) ) ;
#6710 = FACE_OUTER_BOUND ( 'NONE', #12204, .T. ) ;
#6711 = EDGE_CURVE ( 'NONE', #8638, #9434, #3988, .T. ) ;
#6712 = DIRECTION ( 'NONE',  ( -0.9040177279761056894, -0.4274949678123940444, -4.694715627858810513E-16 ) ) ;
#6713 = ADVANCED_FACE ( 'NONE', ( #11097 ), #14397, .F. ) ;
#6714 = DIRECTION ( 'NONE',  ( -1.000000000000000000, 0.000000000000000000, 0.000000000000000000 ) ) ;
#6715 = PLANE ( 'NONE',  #692 ) ;
#6716 = CARTESIAN_POINT ( 'NONE',  ( -7.517426579539127296, -14.72759957212633530, 56.85231026484400019 ) ) ;
#6717 = VERTEX_POINT ( 'NONE', #11018 ) ;
#6718 = CARTESIAN_POINT ( 'NONE',  ( -14.61203582817000246, -106.8625236479798843, -4.516005275576693734 ) ) ;
#6719 = ORIENTED_EDGE ( 'NONE', *, *, #14864, .F. ) ;
#6720 = DIRECTION ( 'NONE',  ( 0.000000000000000000, 0.000000000000000000, 1.000000000000000000 ) ) ;
#6722 = VERTEX_POINT ( 'NONE', #546 ) ;
#6721 = LINE ( 'NONE', #12714, #14739 ) ;
#6723 = ORIENTED_EDGE ( 'NONE', *, *, #10794, .T. ) ;
#6724 = DIRECTION ( 'NONE',  ( 0.5975035461963189576, 0.8018662683283437342, 0.000000000000000000 ) ) ;
#6725 = VERTEX_POINT ( 'NONE', #14465 ) ;
#6726 = AXIS2_PLACEMENT_3D ( 'NONE', #5407, #1977, #9924 ) ;
#6727 = CARTESIAN_POINT ( 'NONE',  ( -10.11292913755864475, -19.52351987967748315, 56.85231026484400019 ) ) ;
#6728 = CARTESIAN_POINT ( 'NONE',  ( -20.87112600995946110, -106.2635794615412834, -5.497689735156005675 ) ) ;
#6729 = SHAPE_REPRESENTATION_RELATIONSHIP ( 'NONE' , 'NONE' ,  #10770, #9362 ) ;
#6730 = EDGE_CURVE ( 'NONE', #12928, #1528, #7019, .T. ) ;
#6731 = ADVANCED_FACE ( 'NONE', ( #8648 ), #1616, .T. ) ;
#6732 = VERTEX_POINT ( 'NONE', #2837 ) ;
#6733 = CARTESIAN_POINT ( 'NONE',  ( -7.797100586692802260, -47.75470106918066193, -7.664321372934788990 ) ) ;
#6734 = FACE_OUTER_BOUND ( 'NONE', #9467, .T. ) ;
#6735 = VERTEX_POINT ( 'NONE', #9729 ) ;
#6736 = LINE ( 'NONE', #10421, #2872 ) ;
#6737 = EDGE_LOOP ( 'NONE', ( #6556, #13077 ) ) ;
#6738 = DIRECTION ( 'NONE',  ( 0.5691548339926102429, 0.8222303661035903488, -3.489949670250048422E-17 ) ) ;
#6739 = EDGE_LOOP ( 'NONE', ( #12318, #6180, #45, #7724, #9946, #10461, #10671, #14847, #8656, #6355, #7832, #9750, #12059, #14895, #13579 ) ) ;
#6740 = ORIENTED_EDGE ( 'NONE', *, *, #7653, .F. ) ;
#6741 = CARTESIAN_POINT ( 'NONE',  ( 2.656674150012286351, -40.75537920817077975, 52.31386353015493285 ) ) ;
#6742 = ORIENTED_EDGE ( 'NONE', *, *, #7381, .F. ) ;
#6744 = EDGE_CURVE ( 'NONE', #14381, #13214, #9877, .T. ) ;
#6743 = DIRECTION ( 'NONE',  ( -0.9578660637129379207, 0.2872152572324145892, -9.396926207859088029E-16 ) ) ;
#6745 = AXIS2_PLACEMENT_3D ( 'NONE', #14614, #5135, #4136 ) ;
#6746 = FACE_OUTER_BOUND ( 'NONE', #7182, .T. ) ;
#6747 = DIRECTION ( 'NONE',  ( -8.018662683283438208E-16, 5.975035461963189015E-16, 1.000000000000000000 ) ) ;
#6748 = CIRCLE ( 'NONE', #185, 9.974999999999999645 ) ;
#6749 = AXIS2_PLACEMENT_3D ( 'NONE', #7228, #12139, #14366 ) ;
#6750 = CARTESIAN_POINT ( 'NONE',  ( -7.586208288801848276, -45.66796403488923772, 21.86702897299116088 ) ) ;
#6752 = DIRECTION ( 'NONE',  ( 0.3190779711151164877, -0.04960027561187742989, -0.9464296386991939425 ) ) ;
#6751 = FACE_OUTER_BOUND ( 'NONE', #14057, .T. ) ;
#6753 = VERTEX_POINT ( 'NONE', #14545 ) ;
#6754 = CARTESIAN_POINT ( 'NONE',  ( -15.49969986081099904, 10.68321993080349763, 24.21206422150099868 ) ) ;
#6755 = AXIS2_PLACEMENT_3D ( 'NONE', #9690, #4957, #9615 ) ;
#6756 = CARTESIAN_POINT ( 'NONE',  ( -17.75434499014690104, -17.41303747754496811, -13.22090772388956914 ) ) ;
#6757 = ORIENTED_EDGE ( 'NONE', *, *, #14408, .T. ) ;
#6758 = ORIENTED_EDGE ( 'NONE', *, *, #5067, .T. ) ;
#6759 = DIRECTION ( 'NONE',  ( -0.8885476655824650072, -0.4587843131450243805, -4.383711467890778149E-16 ) ) ;
#6760 = CARTESIAN_POINT ( 'NONE',  ( -23.43465585259791695, -43.45604609243036265, 56.15319261074063206 ) ) ;
#6761 = CARTESIAN_POINT ( 'NONE',  ( -15.13173615696983099, -107.4889531853311979, -7.801344143962656297 ) ) ;
#6762 = VERTEX_POINT ( 'NONE', #13476 ) ;
#6763 = DIRECTION ( 'NONE',  ( 1.000000000000000000, 1.000000000000000078E-15, 1.000000000000000078E-15 ) ) ;
#6764 = PRODUCT ( 'Slide Locking Screw', 'Slide Locking Screw', '', ( #3835 ) ) ;
#6765 = ADVANCED_FACE ( 'NONE', ( #7496 ), #4062, .F. ) ;
#6766 = CARTESIAN_POINT ( 'NONE',  ( -15.49969986081100437, -101.4268716156739600, -6.728778029351857981 ) ) ;
#6767 = AXIS2_PLACEMENT_3D ( 'NONE', #4178, #8831, #13515 ) ;
#6768 = CARTESIAN_POINT ( 'NONE',  ( -7.499706911750000593, -49.00740941973811005, 19.72872175748142709 ) ) ;
#6769 = VECTOR ( 'NONE', #14508, 1000.000000000000000 ) ;
#6770 = EDGE_CURVE ( 'NONE', #6628, #12018, #6417, .T. ) ;
#6771 = LINE ( 'NONE', #14055, #12116 ) ;
#6772 = CARTESIAN_POINT ( 'NONE',  ( -25.26605094763165127, -15.53691377877616731, 54.00231026484397745 ) ) ;
#6773 = ORIENTED_EDGE ( 'NONE', *, *, #12625, .F. ) ;
#6774 = CARTESIAN_POINT ( 'NONE',  ( -13.79377835810313613, -92.30760736031301406, -0.4016677776517476595 ) ) ;
#6775 = LINE ( 'NONE', #8236, #3125 ) ;
#6776 = CARTESIAN_POINT ( 'NONE',  ( -20.94048570341206883, -6.243833066724571168, 57.00231026484397745 ) ) ;
#6777 = DIRECTION ( 'NONE',  ( -8.018662683283439195E-16, 5.975035461963190001E-16, 1.000000000000000000 ) ) ;
#6778 = VERTEX_POINT ( 'NONE', #6487 ) ;
#6779 = VECTOR ( 'NONE', #8091, 999.9999999999998863 ) ;
#6780 = DIRECTION ( 'NONE',  ( 0.000000000000000000, -1.225619847157526848E-16, 1.000000000000000000 ) ) ;
#6781 = ORIENTED_EDGE ( 'NONE', *, *, #14691, .F. ) ;
#6782 = EDGE_CURVE ( 'NONE', #5603, #10638, #4137, .T. ) ;
#6783 = VECTOR ( 'NONE', #7937, 1000.000000000000000 ) ;
#6784 = CARTESIAN_POINT ( 'NONE',  ( -11.02342383152547178, -36.50737899243796392, 2.502310264844030296 ) ) ;
#6785 = CARTESIAN_POINT ( 'NONE',  ( -13.42547148602778684, -52.23827942061129193, 56.94575044587081436 ) ) ;
#6786 = ADVANCED_FACE ( 'NONE', ( #5282 ), #5068, .F. ) ;
#6787 = FACE_BOUND ( 'NONE', #5881, .T. ) ;
#6788 = CARTESIAN_POINT ( 'NONE',  ( -7.691420491076302213, -11.44776172600821340, 56.85231026484400019 ) ) ;
#6789 = AXIS2_PLACEMENT_3D ( 'NONE', #4381, #12419, #6809 ) ;
#6790 = CARTESIAN_POINT ( 'NONE',  ( -15.61203582816999891, -107.3496051183401647, -7.070526720097524809 ) ) ;
#6791 = DIRECTION ( 'NONE',  ( -0.6780482080269577549, -0.7350174335289139105, -1.045284632676540317E-16 ) ) ;
#6792 = DIRECTION ( 'NONE',  ( 0.000000000000000000, 0.000000000000000000, 1.000000000000000000 ) ) ;
#6793 = DIRECTION ( 'NONE',  ( 8.018662683283438208E-16, -5.975035461963189015E-16, -1.000000000000000000 ) ) ;
#6794 = VERTEX_POINT ( 'NONE', #10696 ) ;
#6795 = CARTESIAN_POINT ( 'NONE',  ( 15.62304162684920428, -29.63692282015450985, 45.13253465925490815 ) ) ;
#6796 = AXIS2_PLACEMENT_3D ( 'NONE', #4146, #8877, #13483 ) ;
#6797 = ORIENTED_EDGE ( 'NONE', *, *, #7474, .T. ) ;
#6799 = VERTEX_POINT ( 'NONE', #1444 ) ;
#6798 = CARTESIAN_POINT ( 'NONE',  ( -5.859109405273535742, -10.94619944609606677, 54.00231026484399166 ) ) ;
#6800 = ORIENTED_EDGE ( 'NONE', *, *, #11375, .F. ) ;
#6801 = PRODUCT_DEFINITION_FORMATION_WITH_SPECIFIED_SOURCE ( 'ANY', '', #11171, .NOT_KNOWN. ) ;
#6802 = ADVANCED_FACE ( 'NONE', ( #3811 ), #6016, .T. ) ;
#6803 = CARTESIAN_POINT ( 'NONE',  ( -15.09158957740191731, -107.1622034095870077, -6.087689735156000204 ) ) ;
#6804 = ADVANCED_FACE ( 'NONE', ( #10778 ), #10627, .F. ) ;
#6805 = ORIENTED_EDGE ( 'NONE', *, *, #6154, .T. ) ;
#6806 = CARTESIAN_POINT ( 'NONE',  ( -19.85327209184728758, -109.9213672076435131, -9.227913261884630458 ) ) ;
#6807 = ADVANCED_FACE ( 'NONE', ( #6242 ), #14298, .T. ) ;
#6808 = DIRECTION ( 'NONE',  ( -8.018662683283438208E-16, 5.975035461963189015E-16, 1.000000000000000000 ) ) ;
#6809 = DIRECTION ( 'NONE',  ( 1.000000000000000000, 0.000000000000000000, 0.000000000000000000 ) ) ;
#6810 = AXIS2_PLACEMENT_3D ( 'NONE', #12646, #12722, #1084 ) ;
#6811 = EDGE_CURVE ( 'NONE', #14409, #470, #8884, .T. ) ;
#6812 = AXIS2_PLACEMENT_3D ( 'NONE', #8825, #5388, #2870 ) ;
#6813 = ORIENTED_EDGE ( 'NONE', *, *, #393, .F. ) ;
#6814 = FACE_BOUND ( 'NONE', #722, .T. ) ;
#6815 = EDGE_LOOP ( 'NONE', ( #6255, #2674, #5885, #14335, #8165, #5532, #12546, #6282 ) ) ;
#6816 = CARTESIAN_POINT ( 'NONE',  ( 14.77462936471488142, -26.10186736074272673, 46.34164862513579664 ) ) ;
#6817 = VERTEX_POINT ( 'NONE', #1287 ) ;
#6818 =( BOUNDED_CURVE ( )  B_SPLINE_CURVE ( 3, ( #11656, #1036, #12509, #1104 ),
 .UNSPECIFIED., .F., .F. ) 
 B_SPLINE_CURVE_WITH_KNOTS ( ( 4, 4 ),
 ( 4.712388980384689674, 6.283185307179586232 ),
 .UNSPECIFIED. ) 
 CURVE ( )  GEOMETRIC_REPRESENTATION_ITEM ( )  RATIONAL_B_SPLINE_CURVE ( ( 1.000000000000000000, 0.8047378541243649375, 0.8047378541243649375, 1.000000000000000000 ) ) 
 REPRESENTATION_ITEM ( '' )  );
#6819 = FACE_OUTER_BOUND ( 'NONE', #10189, .T. ) ;
#6820 = ORIENTED_EDGE ( 'NONE', *, *, #1882, .T. ) ;
#6821 = VERTEX_POINT ( 'NONE', #8474 ) ;
#6822 = EDGE_CURVE ( 'NONE', #280, #3379, #9626, .T. ) ;
#6823 = CARTESIAN_POINT ( 'NONE',  ( -18.09969986081100046, -107.2302401527028337, -7.385908130336948929 ) ) ;
#6824 = EDGE_CURVE ( 'NONE', #10152, #11272, #13234, .T. ) ;
#6825 = ORIENTED_EDGE ( 'NONE', *, *, #5500, .F. ) ;
#6826 = VECTOR ( 'NONE', #4323, 1000.000000000000000 ) ;
#6827 = CARTESIAN_POINT ( 'NONE',  ( -7.499699860810998153, -43.98402112729824864, 56.13904046828872652 ) ) ;
#6828 = B_SPLINE_CURVE_WITH_KNOTS ( 'NONE', 3,
 ( #7079, #13078, #4809, #1210, #3736, #7318 ),
 .UNSPECIFIED., .F., .F.,
 ( 4, 2, 4 ),
 ( 0.000000000000000000, 0.1441277441444622220, 0.2882554882889244441 ),
 .UNSPECIFIED. ) ;
#6829 = DIRECTION ( 'NONE',  ( 0.000000000000000000, -2.168404344971008868E-16, 1.000000000000000000 ) ) ;
#6830 = DIRECTION ( 'NONE',  ( 8.018662683283438208E-16, -5.975035461963189015E-16, -1.000000000000000000 ) ) ;
#6831 = EDGE_CURVE ( 'NONE', #3128, #11105, #11360, .T. ) ;
#6832 = CARTESIAN_POINT ( 'NONE',  ( -13.02562488396841900, -21.19439421350821817, 57.00231026484399166 ) ) ;
#6834 = FACE_OUTER_BOUND ( 'NONE', #4128, .T. ) ;
#6833 = CARTESIAN_POINT ( 'NONE',  ( -10.08476707729037258, -21.88467736064467672, 54.00231026484400587 ) ) ;
#6835 = VERTEX_POINT ( 'NONE', #7165 ) ;
#6836 = CARTESIAN_POINT ( 'NONE',  ( -15.45378054160984682, -13.48759475315262613, 56.85231026484398598 ) ) ;
#6837 = ORIENTED_EDGE ( 'NONE', *, *, #9266, .T. ) ;
#6838 = ORIENTED_EDGE ( 'NONE', *, *, #14300, .T. ) ;
#6839 = CARTESIAN_POINT ( 'NONE',  ( -34.99969986081099904, -19.50737899243800300, 51.22375411596780026 ) ) ;
#6840 = CARTESIAN_POINT ( 'NONE',  ( -15.49969986081092088, -13.50737899243822504, 57.00231026484397745 ) ) ;
#6841 = PLANE ( 'NONE',  #9130 ) ;
#6842 = ORIENTED_EDGE ( 'NONE', *, *, #4592, .F. ) ;
#6843 = DIRECTION ( 'NONE',  ( -0.9645173894937556502, -0.2640193276336997297, -6.156614753256502225E-16 ) ) ;
#6844 = EDGE_CURVE ( 'NONE', #13647, #4255, #7083, .T. ) ;
#6845 = CARTESIAN_POINT ( 'NONE',  ( -15.61203582817000068, -106.2173407584721616, -5.758565883178085265 ) ) ;
#6846 = CARTESIAN_POINT ( 'NONE',  ( -6.488891646287396675, -12.42729319905174634, 56.85231026484400019 ) ) ;
#6847 = EDGE_CURVE ( 'NONE', #14890, #8709, #11847, .T. ) ;
#6848 = EDGE_CURVE ( 'NONE', #2925, #8256, #2741, .T. ) ;
#6849 = DIRECTION ( 'NONE',  ( -0.5975035461963188466, -0.8018662683283437342, 0.000000000000000000 ) ) ;
#6850 = LINE ( 'NONE', #3498, #8901 ) ;
#6851 = ORIENTED_EDGE ( 'NONE', *, *, #2242, .F. ) ;
#6852 = CARTESIAN_POINT ( 'NONE',  ( -13.36723182930882103, -91.92030416804652759, -0.5674792550076069864 ) ) ;
#6853 = CARTESIAN_POINT ( 'NONE',  ( -35.68452948511416167, 6.083222336789435580, 29.65309064885218859 ) ) ;
#6854 = DIRECTION ( 'NONE',  ( 1.049727191138615861E-16, 0.5150380749100581523, -0.8571673007021098911 ) ) ;
#6855 = ORIENTED_EDGE ( 'NONE', *, *, #13693, .T. ) ;
#6856 = LINE ( 'NONE', #14909, #13778 ) ;
#6857 = ORIENTED_EDGE ( 'NONE', *, *, #7323, .T. ) ;
#6858 = AXIS2_PLACEMENT_3D ( 'NONE', #5086, #12050, #1563 ) ;
#6859 = CARTESIAN_POINT ( 'NONE',  ( -7.517426579539127296, -14.72759957212633530, 57.00231026484399166 ) ) ;
#6860 = CARTESIAN_POINT ( 'NONE',  ( -18.93133274217424855, -21.90887563098697655, 56.85231026484400019 ) ) ;
#6861 = LINE ( 'NONE', #1216, #309 ) ;
#6862 = CARTESIAN_POINT ( 'NONE',  ( -1.508527451664997798, -48.23942980000687442, -5.497689735155999458 ) ) ;
#6863 = DIRECTION ( 'NONE',  ( 1.000000000000000000, -1.291538348938060198E-32, 1.054621095516909827E-16 ) ) ;
#6864 = AXIS2_PLACEMENT_3D ( 'NONE', #3597, #3443, #1144 ) ;
#6865 = ADVANCED_FACE ( 'NONE', ( #14221 ), #13082, .T. ) ;
#6866 = CARTESIAN_POINT ( 'NONE',  ( -8.858895634567669930, -20.95051974273373929, 57.00231026484399166 ) ) ;
#6867 = DIRECTION ( 'NONE',  ( -8.018662683283438208E-16, 5.975035461963189015E-16, 1.000000000000000000 ) ) ;
#6868 = CARTESIAN_POINT ( 'NONE',  ( -2.216578225681298697, -31.14135358865360104, -10.85656391856669778 ) ) ;
#6869 = ORIENTED_EDGE ( 'NONE', *, *, #11984, .T. ) ;
#6870 = CARTESIAN_POINT ( 'NONE',  ( -15.61203582817000068, -106.9373417306329515, -4.908392192767063733 ) ) ;
#6871 = ORIENTED_EDGE ( 'NONE', *, *, #12653, .F. ) ;
#6873 = VERTEX_POINT ( 'NONE', #7237 ) ;
#6872 = CARTESIAN_POINT ( 'NONE',  ( -15.49969986081086226, -13.50737899243826767, -13.99768973515600301 ) ) ;
#6874 = VERTEX_POINT ( 'NONE', #7320 ) ;
#6875 = AXIS2_PLACEMENT_3D ( 'NONE', #9886, #13416, #13269 ) ;
#6876 = PLANE ( 'NONE',  #11178 ) ;
#6877 = VERTEX_POINT ( 'NONE', #12003 ) ;
#6878 = VECTOR ( 'NONE', #8318, 1000.000000000000000 ) ;
#6879 = CIRCLE ( 'NONE', #5187, 22.99999999999999645 ) ;
#6880 = DIRECTION ( 'NONE',  ( 1.000000000000000000, 1.201369187114119994E-15, 9.616040805000176517E-16 ) ) ;
#6881 = AXIS2_PLACEMENT_3D ( 'NONE', #616, #13399, #6635 ) ;
#6882 = CARTESIAN_POINT ( 'NONE',  ( -7.223083447440863836, -17.23012942000294245, 56.85231026484400019 ) ) ;
#6883 = ADVANCED_FACE ( 'NONE', ( #1519 ), #6174, .F. ) ;
#6884 = AXIS2_PLACEMENT_3D ( 'NONE', #1249, #5904, #265 ) ;
#6885 = AXIS2_PLACEMENT_3D ( 'NONE', #1393, #2469, #11798 ) ;
#6886 = CARTESIAN_POINT ( 'NONE',  ( -22.67629672040707334, -48.05217323185801348, -17.30478718853205322 ) ) ;
#6887 = EDGE_CURVE ( 'NONE', #1247, #14370, #12724, .T. ) ;
#6888 = VERTEX_POINT ( 'NONE', #2006 ) ;
#6889 = CARTESIAN_POINT ( 'NONE',  ( -10.11292913755864475, -19.52351987967748315, 56.85231026484400019 ) ) ;
#6890 = VERTEX_POINT ( 'NONE', #5443 ) ;
#6891 = CARTESIAN_POINT ( 'NONE',  ( -23.49969986081099904, -19.50737899243800300, 48.00231026484399877 ) ) ;
#6892 = VERTEX_POINT ( 'NONE', #2234 ) ;
#6893 = ORIENTED_EDGE ( 'NONE', *, *, #12945, .T. ) ;
#6894 = LINE ( 'NONE', #5682, #2734 ) ;
#6895 = ORIENTED_EDGE ( 'NONE', *, *, #9247, .F. ) ;
#6896 = EDGE_CURVE ( 'NONE', #5522, #12480, #6656, .T. ) ;
#6897 = CARTESIAN_POINT ( 'NONE',  ( -21.33331128615267858, -21.63851970382446055, 56.54902971347384266 ) ) ;
#6898 = VECTOR ( 'NONE', #3376, 1000.000000000000114 ) ;
#6899 = DIRECTION ( 'NONE',  ( 0.000000000000000000, 0.000000000000000000, -1.000000000000000000 ) ) ;
#6900 = DIRECTION ( 'NONE',  ( 0.000000000000000000, 1.000000000000000000, 1.224646799147350002E-16 ) ) ;
#6901 = EDGE_CURVE ( 'NONE', #9153, #7447, #5520, .T. ) ;
#6902 = ADVANCED_FACE ( 'NONE', ( #9343 ), #249, .T. ) ;
#6903 = LINE ( 'NONE', #2029, #837 ) ;
#6905 = DIRECTION ( 'NONE',  ( 0.000000000000000000, 0.000000000000000000, 1.000000000000000000 ) ) ;
#6904 = CARTESIAN_POINT ( 'NONE',  ( -9.959408463899002584, -21.80230492564002276, 56.85231026484400019 ) ) ;
#6906 = ORIENTED_EDGE ( 'NONE', *, *, #4003, .T. ) ;
#6907 = LINE ( 'NONE', #3261, #11192 ) ;
#6908 = DIRECTION ( 'NONE',  ( 0.5975035461963188466, 0.8018662683283437342, 0.000000000000000000 ) ) ;
#6909 = ORIENTED_EDGE ( 'NONE', *, *, #8063, .F. ) ;
#6910 = ORIENTED_EDGE ( 'NONE', *, *, #8399, .F. ) ;
#6911 = CYLINDRICAL_SURFACE ( 'NONE', #7860, 0.2000000000000012046 ) ;
#6912 = VECTOR ( 'NONE', #12853, 1000.000000000000000 ) ;
#6913 = CARTESIAN_POINT ( 'NONE',  ( -15.49969986081099904, -57.00737899243800655, -5.497689735156002122 ) ) ;
#6914 = CARTESIAN_POINT ( 'NONE',  ( -11.95055483344002312, -37.31872034517681413, -17.83250243206357410 ) ) ;
#6915 = ORIENTED_EDGE ( 'NONE', *, *, #3938, .F. ) ;
#6916 = CARTESIAN_POINT ( 'NONE',  ( -7.264457220180047692, -15.89840986842768977, 57.00231026484399166 ) ) ;
#6917 = CARTESIAN_POINT ( 'NONE',  ( -20.06719866676104402, -21.34952185377683165, 57.00231026484397745 ) ) ;
#6918 = ITEM_DEFINED_TRANSFORMATION ( 'NONE', 'NONE', #2425,  #6789 ) ;
#6919 =( GEOMETRIC_REPRESENTATION_CONTEXT ( 3 ) GLOBAL_UNCERTAINTY_ASSIGNED_CONTEXT ( ( #11988 ) ) GLOBAL_UNIT_ASSIGNED_CONTEXT ( ( #14278, #1265, #208 ) ) REPRESENTATION_CONTEXT ( 'NONE', 'WORKASPACE' ) );
#6920 = LINE ( 'NONE', #8230, #7986 ) ;
#6921 = EDGE_CURVE ( 'NONE', #1753, #3679, #9496, .T. ) ;
#6922 = CARTESIAN_POINT ( 'NONE',  ( -7.501950027729723303, -44.50597529135383468, 20.99749114769749880 ) ) ;
#6923 = DIRECTION ( 'NONE',  ( 0.3204693369899919708, 0.9472588896649083434, -3.090169943749469383E-16 ) ) ;
#6924 = EDGE_LOOP ( 'NONE', ( #11999, #4965, #3301, #11440 ) ) ;
#6925 = CARTESIAN_POINT ( 'NONE',  ( -35.90391930765986928, 5.977956585851525340, 29.53688810851901181 ) ) ;
#6926 = VECTOR ( 'NONE', #5358, 999.9999999999998863 ) ;
#6927 = LINE ( 'NONE', #3201, #7172 ) ;
#6928 = DIRECTION ( 'NONE',  ( -8.018662683283438208E-16, 5.975035461963189015E-16, 1.000000000000000000 ) ) ;
#6929 = ORIENTED_EDGE ( 'NONE', *, *, #8116, .T. ) ;
#6930 = CARTESIAN_POINT ( 'NONE',  ( -7.704540658288731692, -46.31685722003375361, 47.00231026484399166 ) ) ;
#6931 = EDGE_LOOP ( 'NONE', ( #9546, #2308 ) ) ;
#6932 = VECTOR ( 'NONE', #12535, 1000.000000000000000 ) ;
#6933 = DIRECTION ( 'NONE',  ( -8.018662683283438208E-16, 5.975035461963189015E-16, 1.000000000000000000 ) ) ;
#6934 = DIRECTION ( 'NONE',  ( -1.000000000000000000, 1.291538348938060198E-32, -1.054621095516909827E-16 ) ) ;
#6935 = ADVANCED_FACE ( 'NONE', ( #173 ), #10494, .T. ) ;
#6936 = DIRECTION ( 'NONE',  ( -8.018662683283439195E-16, 5.975035461963190001E-16, 1.000000000000000000 ) ) ;
#6937 = FACE_BOUND ( 'NONE', #13453, .T. ) ;
#6938 = VECTOR ( 'NONE', #1, 1000.000000000000000 ) ;
#6939 = CARTESIAN_POINT ( 'NONE',  ( 14.68618260102866913, -27.00737899243800300, 1.962064221501000683 ) ) ;
#6940 = CARTESIAN_POINT ( 'NONE',  ( -8.600581100527527667, -9.311215824554304632, 57.00231026484399166 ) ) ;
#6941 = DIRECTION ( 'NONE',  ( 1.000000000000000000, 1.201369187114119994E-15, 9.616040805000176517E-16 ) ) ;
#6942 = ORIENTED_EDGE ( 'NONE', *, *, #10633, .F. ) ;
#6943 = DIRECTION ( 'NONE',  ( 0.9578660637129379207, -0.2872152572324145892, 9.396926207859088029E-16 ) ) ;
#6944 = ORIENTED_EDGE ( 'NONE', *, *, #14487, .T. ) ;
#6946 = VERTEX_POINT ( 'NONE', #1086 ) ;
#6945 = CARTESIAN_POINT ( 'NONE',  ( -22.10635852801940260, -5.970339595447221370, 61.12849997418209114 ) ) ;
#6947 = ORIENTED_EDGE ( 'NONE', *, *, #9826, .F. ) ;
#6948 = CARTESIAN_POINT ( 'NONE',  ( -24.55043086433169819, -12.83990741858047357, 56.85231026484398598 ) ) ;
#6949 = ORIENTED_EDGE ( 'NONE', *, *, #13922, .T. ) ;
#6950 = LINE ( 'NONE', #5817, #13184 ) ;
#6951 = EDGE_CURVE ( 'NONE', #9250, #6353, #4533, .T. ) ;
#6952 = LINE ( 'NONE', #3454, #13332 ) ;
#6953 = DIRECTION ( 'NONE',  ( 0.9957106782009863544, 0.09252159378508258147, 7.431448254773871651E-16 ) ) ;
#6954 = CARTESIAN_POINT ( 'NONE',  ( 15.03594476211659270, -25.29111237089811581, 2.444031612587182156 ) ) ;
#6955 = DIRECTION ( 'NONE',  ( 1.000000000000000000, 1.201369187114119994E-15, 9.616040805000176517E-16 ) ) ;
#6956 = ORIENTED_EDGE ( 'NONE', *, *, #7802, .F. ) ;
#6957 = CARTESIAN_POINT ( 'NONE',  ( 7.203956337210061456, -37.00737899243799944, -10.34622021768276667 ) ) ;
#6958 = ORIENTED_EDGE ( 'NONE', *, *, #3691, .F. ) ;
#6959 = AXIS2_PLACEMENT_3D ( 'NONE', #11378, #6698, #14598 ) ;
#6960 = CARTESIAN_POINT ( 'NONE',  ( -1.508527451664999575, -45.64135358865355130, -6.997689735156000346 ) ) ;
#6961 = ORIENTED_EDGE ( 'NONE', *, *, #12248, .F. ) ;
#6962 = VERTEX_POINT ( 'NONE', #14014 ) ;
#6963 = CARTESIAN_POINT ( 'NONE',  ( 4.127468730679389353, -38.31628777932305496, 51.45578572424146557 ) ) ;
#6964 = ORIENTED_EDGE ( 'NONE', *, *, #2961, .F. ) ;
#6965 = LINE ( 'NONE', #7281, #12532 ) ;
#6966 = EDGE_CURVE ( 'NONE', #3490, #505, #6952, .T. ) ;
#6967 = EDGE_CURVE ( 'NONE', #12833, #7723, #12804, .T. ) ;
#6968 = DIRECTION ( 'NONE',  ( 1.000000000000000000, 0.000000000000000000, 0.000000000000000000 ) ) ;
#6969 = CARTESIAN_POINT ( 'NONE',  ( -10.12903334873179517, -90.53886212111028442, -5.595198070896032938 ) ) ;
#6970 = B_SPLINE_CURVE_WITH_KNOTS ( 'NONE', 3,
 ( #9547, #3091, #7603, #1801 ),
 .UNSPECIFIED., .F., .F.,
 ( 4, 4 ),
 ( 0.8772494290945609396, 1.000000000000000000 ),
 .UNSPECIFIED. ) ;
#6971 = CARTESIAN_POINT ( 'NONE',  ( -7.507587349371155128, -44.88838417754359966, 21.40739837630950504 ) ) ;
#6973 = DIRECTION ( 'NONE',  ( -8.018662683283438208E-16, 5.975035461963189015E-16, 1.000000000000000000 ) ) ;
#6972 = DIRECTION ( 'NONE',  ( 0.5975035461963189576, 0.8018662683283437342, 0.000000000000000000 ) ) ;
#6974 = VERTEX_POINT ( 'NONE', #11636 ) ;
#6975 = DIRECTION ( 'NONE',  ( 0.9183863840214728791, 0.3956847857120156520, 4.999999999999998416E-16 ) ) ;
#6976 = CARTESIAN_POINT ( 'NONE',  ( -17.49270643681038706, -17.55260497673067732, -13.23591867084377327 ) ) ;
#6977 = EDGE_LOOP ( 'NONE', ( #8744, #6518, #8710, #12368 ) ) ;
#6978 = VERTEX_POINT ( 'NONE', #1155 ) ;
#6979 = DIRECTION ( 'NONE',  ( 1.169602638241521591E-15, -0.1872998510044552312, -0.9823027872370662106 ) ) ;
#6980 = DIRECTION ( 'NONE',  ( -0.9999272109403024578, 0.01206535623791937274, -8.090169943749475688E-16 ) ) ;
#6981 = CIRCLE ( 'NONE', #6018, 23.00000000000000000 ) ;
#6982 = ORIENTED_EDGE ( 'NONE', *, *, #13441, .T. ) ;
#6983 = CARTESIAN_POINT ( 'NONE',  ( -7.499699860810999041, -44.50737899243799944, -17.13441993860073964 ) ) ;
#6984 = ORIENTED_EDGE ( 'NONE', *, *, #10180, .T. ) ;
#6985 = EDGE_CURVE ( 'NONE', #13132, #10963, #2391, .T. ) ;
#6986 = ADVANCED_FACE ( 'NONE', ( #9569 ), #5746, .T. ) ;
#6987 = MECHANICAL_DESIGN_GEOMETRIC_PRESENTATION_REPRESENTATION (  '', ( #13611 ), #14357 ) ;
#6988 = EDGE_CURVE ( 'NONE', #3638, #3090, #6542, .T. ) ;
#6989 = CYLINDRICAL_SURFACE ( 'NONE', #11968, 0.2000000000000012046 ) ;
#6990 = CARTESIAN_POINT ( 'NONE',  ( -18.10194853779420399, -23.13696500758646835, 57.00231026484399166 ) ) ;
#6991 = EDGE_CURVE ( 'NONE', #10870, #8351, #4760, .T. ) ;
#6992 = CARTESIAN_POINT ( 'NONE',  ( -38.49969986081099904, -37.00737899243799944, 52.39987856403599409 ) ) ;
#6993 = CARTESIAN_POINT ( 'NONE',  ( -37.04494295528539993, 20.99262100756200056, 16.16206422150100153 ) ) ;
#6994 = ORIENTED_EDGE ( 'NONE', *, *, #4157, .F. ) ;
#6995 = DIRECTION ( 'NONE',  ( -0.6780482080269607525, -0.7350174335289111349, -1.045284632676580746E-16 ) ) ;
#6996 = CARTESIAN_POINT ( 'NONE',  ( -35.90397664832814684, 5.977929128642675671, 29.53685653062469640 ) ) ;
#6997 = PLANE ( 'NONE',  #12814 ) ;
#6998 = VECTOR ( 'NONE', #8942, 1000.000000000000000 ) ;
#6999 = DIRECTION ( 'NONE',  ( -8.018662683283438208E-16, 5.975035461963189015E-16, 1.000000000000000000 ) ) ;
#7000 = ORIENTED_EDGE ( 'NONE', *, *, #12080, .T. ) ;
#7001 = CARTESIAN_POINT ( 'NONE',  ( -12.95836108888110516, -12.41244868326982953, 51.00231026484399166 ) ) ;
#7002 = ORIENTED_EDGE ( 'NONE', *, *, #11138, .F. ) ;
#7003 = PLANE ( 'NONE',  #552 ) ;
#7004 = FACE_BOUND ( 'NONE', #11820, .T. ) ;
#7005 = ADVANCED_FACE ( 'NONE', ( #13033 ), #13940, .F. ) ;
#7006 = AXIS2_PLACEMENT_3D ( 'NONE', #1125, #8074, #2127 ) ;
#7007 = VECTOR ( 'NONE', #2461, 1000.000000000000000 ) ;
#7008 = DIRECTION ( 'NONE',  ( -2.940315329303969755E-16, 0.8386705679454240503, -0.5446390350150269732 ) ) ;
#7009 = CARTESIAN_POINT ( 'NONE',  ( -11.02342383152546645, -36.50737899243797102, 11.50231026484397034 ) ) ;
#7010 = B_SPLINE_CURVE_WITH_KNOTS ( 'NONE', 3,
 ( #4386, #9039, #2091, #14074, #3517, #6580, #944, #12344, #9406, #6733, #11265, #4668, #9324, #12861, #2376, #7013, #1862, #5873, #2786, #10592, #14268, #7288, #7441, #6063, #8592, #4864, #1412, #9517, #125, #3785, #424, #2562, #7210, #6136, #1255, #5913, #8365, #10745, #10823, #6217, #11890, #14111, #4785, #4935, #1490, #272, #8286, #14344, #9442 ),
 .UNSPECIFIED., .F., .F.,
 ( 4, 2, 2, 1, 1, 2, 2, 2, 2, 1, 1, 2, 2, 2, 2, 2, 1, 2, 2, 2, 2, 2, 1, 1, 2, 2, 2, 4 ),
 ( 0.000000000000000000, 0.06250000000000491274, 0.09375000000000881240, 0.1093750000000107969, 0.1171875000000118239, 0.1210937500000123374, 0.1250000000000128508, 0.1875000000000081324, 0.2187500000000046074, 0.2343750000000028866, 0.2421875000000020539, 0.2460937500000008049, 0.2499999999999995559, 0.3750000000000037192, 0.4375000000000054401, 0.4687500000000063838, 0.4843750000000064948, 0.4921875000000063283, 0.5000000000000061062, 0.6250000000000033307, 0.6875000000000025535, 0.7187500000000021094, 0.7343750000000025535, 0.7421875000000033307, 0.7460937500000037748, 0.7500000000000042188, 0.8750000000000021094, 1.000000000000000000 ),
 .UNSPECIFIED. ) ;
#7011 = DIRECTION ( 'NONE',  ( -0.9225966037272086417, 0.3857661296576204712, -9.702957262759976898E-16 ) ) ;
#7012 = CARTESIAN_POINT ( 'NONE',  ( 7.000300139189000070, -19.50737899243800300, 24.21206422150099868 ) ) ;
#7013 = CARTESIAN_POINT ( 'NONE',  ( -7.690624001723991299, -48.30857337213005565, -7.231759084041137875 ) ) ;
#7014 = CIRCLE ( 'NONE', #452, 9.974999999999999645 ) ;
#7015 = AXIS2_PLACEMENT_3D ( 'NONE', #200, #5993, #9520 ) ;
#7016 = CARTESIAN_POINT ( 'NONE',  ( -35.59468245696151456, -37.93213861349480709, 51.16428679575325589 ) ) ;
#7017 = EDGE_CURVE ( 'NONE', #12259, #11477, #8264, .T. ) ;
#7018 = CARTESIAN_POINT ( 'NONE',  ( -24.33650094517379614, -11.44044972528773130, 57.00231026484397745 ) ) ;
#7019 = CIRCLE ( 'NONE', #12418, 10.00000000000000000 ) ;
#7020 = EDGE_LOOP ( 'NONE', ( #4291, #13042, #13719, #14334 ) ) ;
#7021 = FACE_OUTER_BOUND ( 'NONE', #7119, .T. ) ;
#7022 = ORIENTED_EDGE ( 'NONE', *, *, #7342, .F. ) ;
#7024 = VERTEX_POINT ( 'NONE', #14246 ) ;
#7023 = DIRECTION ( 'NONE',  ( 0.4800904676395372217, 0.8772189822852960450, -1.391731009600650064E-16 ) ) ;
#7025 = ORIENTED_EDGE ( 'NONE', *, *, #11311, .T. ) ;
#7026 = CARTESIAN_POINT ( 'NONE',  ( -7.424382730750141768, -13.52981220323889566, 57.00231026484399166 ) ) ;
#7027 = ORIENTED_EDGE ( 'NONE', *, *, #503, .T. ) ;
#7028 = AXIS2_PLACEMENT_3D ( 'NONE', #6437, #13421, #6213 ) ;
#7029 = DIRECTION ( 'NONE',  ( 1.054621095516909827E-16, 1.224646799147350002E-16, -1.000000000000000000 ) ) ;
#7030 = DIRECTION ( 'NONE',  ( 0.000000000000000000, -1.000000000000000000, -1.224646799147350002E-16 ) ) ;
#7031 = DIRECTION ( 'NONE',  ( 1.000000000000000078E-15, 0.000000000000000000, -1.000000000000000000 ) ) ;
#7032 = DIRECTION ( 'NONE',  ( 1.000000000000000000, 0.000000000000000000, 0.000000000000000000 ) ) ;
#7033 = CARTESIAN_POINT ( 'NONE',  ( -7.499699860810999041, -44.50737899243799944, 43.00231026484400587 ) ) ;
#7034 = CARTESIAN_POINT ( 'NONE',  ( -15.13173615696983276, -107.1622034095870077, -6.087689735156000204 ) ) ;
#7035 =( BOUNDED_CURVE ( )  B_SPLINE_CURVE ( 3, ( #8066, #14742, #11445, #4341 ),
 .UNSPECIFIED., .F., .F. ) 
 B_SPLINE_CURVE_WITH_KNOTS ( ( 4, 4 ),
 ( 5.550165736622670209, 6.177741627597179708 ),
 .UNSPECIFIED. ) 
 CURVE ( )  GEOMETRIC_REPRESENTATION_ITEM ( )  RATIONAL_B_SPLINE_CURVE ( ( 1.000000000000000000, 0.9674474632520878581, 0.9674474632520878581, 1.000000000000000000 ) ) 
 REPRESENTATION_ITEM ( '' )  );
#7036 = VECTOR ( 'NONE', #8207, 1000.000000000000114 ) ;
#7037 = EDGE_CURVE ( 'NONE', #10921, #33, #7107, .T. ) ;
#7038 = PLANE ( 'NONE',  #10821 ) ;
#7039 = ORIENTED_EDGE ( 'NONE', *, *, #2981, .F. ) ;
#7040 = CARTESIAN_POINT ( 'NONE',  ( 2.995488256399623239, -39.83604612058397976, -13.11945893988026413 ) ) ;
#7041 = EDGE_LOOP ( 'NONE', ( #574, #9657, #2228, #8641 ) ) ;
#7042 = SURFACE_STYLE_USAGE ( .BOTH. , #258 ) ;
#7043 = ORIENTED_EDGE ( 'NONE', *, *, #6831, .T. ) ;
#7044 = B_SPLINE_CURVE_WITH_KNOTS ( 'NONE', 3,
 ( #3962, #521, #14591, #14372 ),
 .UNSPECIFIED., .F., .F.,
 ( 4, 4 ),
 ( 0.000000000000000000, 0.1210918566152707487 ),
 .UNSPECIFIED. ) ;
#7045 = ORIENTED_EDGE ( 'NONE', *, *, #788, .T. ) ;
#7046 = DIRECTION ( 'NONE',  ( 8.018662683283438208E-16, -5.975035461963189015E-16, -1.000000000000000000 ) ) ;
#7047 = ORIENTED_EDGE ( 'NONE', *, *, #743, .T. ) ;
#7048 = DIRECTION ( 'NONE',  ( 0.9931883319083343320, -0.1165201156931293391, 8.660254037844387408E-16 ) ) ;
#7049 = CIRCLE ( 'NONE', #7537, 9.974999999999999645 ) ;
#7050 = PRODUCT_DEFINITION_FORMATION_WITH_SPECIFIED_SOURCE ( 'ANY', '', #6764, .NOT_KNOWN. ) ;
#7051 = DIRECTION ( 'NONE',  ( 7.070501591499390115E-17, -1.224646799147350002E-16, 1.000000000000000000 ) ) ;
#7052 = CARTESIAN_POINT ( 'NONE',  ( -11.39494938265116453, -90.81200083036684134, -8.981479305044373973 ) ) ;
#7053 = CARTESIAN_POINT ( 'NONE',  ( -15.49969986081099904, -32.00737899243799944, 24.21206422150099868 ) ) ;
#7054 = EDGE_CURVE ( 'NONE', #11046, #10705, #545, .T. ) ;
#7056 = CARTESIAN_POINT ( 'NONE',  ( -38.36092261288197136, 4.383170266566359885, 26.75226997007207075 ) ) ;
#7055 = CYLINDRICAL_SURFACE ( 'NONE', #2535, 4.499999999999999112 ) ;
#7057 = ORIENTED_EDGE ( 'NONE', *, *, #4943, .F. ) ;
#7058 = CARTESIAN_POINT ( 'NONE',  ( -15.49969986081099904, -27.00737899243800300, -5.497689735156002122 ) ) ;
#7059 = LINE ( 'NONE', #3262, #14504 ) ;
#7060 = ORIENTED_EDGE ( 'NONE', *, *, #1585, .T. ) ;
#7061 = VECTOR ( 'NONE', #12528, 1000.000000000000114 ) ;
#7062 = CARTESIAN_POINT ( 'NONE',  ( -23.23036473679183445, -42.43240574409319521, 56.19689949488600433 ) ) ;
#7063 = ORIENTED_EDGE ( 'NONE', *, *, #10301, .F. ) ;
#7064 = ORIENTED_EDGE ( 'NONE', *, *, #12664, .T. ) ;
#7065 = CARTESIAN_POINT ( 'NONE',  ( -15.49969986081099904, 71.39262100756199914, 15.89786062077516782 ) ) ;
#7066 = CONTEXT_DEPENDENT_SHAPE_REPRESENTATION ( #1953, #12395 ) ;
#7067 = LINE ( 'NONE', #13902, #9475 ) ;
#7068 = DIRECTION ( 'NONE',  ( 8.018662683283438208E-16, -5.975035461963189015E-16, -1.000000000000000000 ) ) ;
#7069 = EDGE_CURVE ( 'NONE', #15017, #9709, #1316, .T. ) ;
#7070 = DIRECTION ( 'NONE',  ( -0.1165201156931293391, -0.9931883319083343320, 4.999999999999998416E-16 ) ) ;
#7072 = ORIENTED_EDGE ( 'NONE', *, *, #10463, .T. ) ;
#7071 = VECTOR ( 'NONE', #2236, 1000.000000000000000 ) ;
#7073 = CARTESIAN_POINT ( 'NONE',  ( -15.49969986081092088, -13.50737899243822504, 56.85231026484398598 ) ) ;
#7074 = CARTESIAN_POINT ( 'NONE',  ( -15.49969986081100082, 22.99262100756200411, 8.337064221501000461 ) ) ;
#7075 = ORIENTED_EDGE ( 'NONE', *, *, #3838, .T. ) ;
#7076 = EDGE_CURVE ( 'NONE', #11595, #9643, #9873, .T. ) ;
#7077 = CARTESIAN_POINT ( 'NONE',  ( -27.49969986081100259, -57.00737899243800655, 19.50231026484398811 ) ) ;
#7078 = ORIENTED_EDGE ( 'NONE', *, *, #14406, .F. ) ;
#7079 = CARTESIAN_POINT ( 'NONE',  ( -7.512805849530849400, -44.04964101872670312, -5.955427708867301106 ) ) ;
#7080 = ORIENTED_EDGE ( 'NONE', *, *, #5740, .F. ) ;
#7081 = CARTESIAN_POINT ( 'NONE',  ( -15.49969986081091200, -13.50737899243823215, 48.00231026484398456 ) ) ;
#7082 = CARTESIAN_POINT ( 'NONE',  ( -19.05456510292772521, -4.187316862259579331, 54.00231026484397745 ) ) ;
#7083 = LINE ( 'NONE', #8395, #137 ) ;
#7084 = ADVANCED_FACE ( 'NONE', ( #7341 ), #6113, .F. ) ;
#7085 = CARTESIAN_POINT ( 'NONE',  ( -23.08034316846174150, -10.72437754756471762, 56.85231026484398598 ) ) ;
#7086 = DIRECTION ( 'NONE',  ( 0.000000000000000000, 0.000000000000000000, -1.000000000000000000 ) ) ;
#7087 = CARTESIAN_POINT ( 'NONE',  ( -6.405052749715342664, -17.67073240653434496, 60.59267971125725438 ) ) ;
#7088 = EDGE_CURVE ( 'NONE', #13469, #13305, #8434, .T. ) ;
#7089 = LINE ( 'NONE', #5652, #10412 ) ;
#7090 = EDGE_CURVE ( 'NONE', #1539, #11046, #9651, .T. ) ;
#7091 = ORIENTED_EDGE ( 'NONE', *, *, #9245, .F. ) ;
#7092 = LINE ( 'NONE', #11775, #11416 ) ;
#7093 = EDGE_CURVE ( 'NONE', #7312, #4342, #3308, .T. ) ;
#7094 = FACE_OUTER_BOUND ( 'NONE', #7798, .T. ) ;
#7095 = VECTOR ( 'NONE', #5449, 1000.000000000000000 ) ;
#7096 = CARTESIAN_POINT ( 'NONE',  ( -20.45368390747784204, -7.130130991507916072, 57.00231026484397745 ) ) ;
#7097 = ORIENTED_EDGE ( 'NONE', *, *, #7069, .F. ) ;
#7098 = CARTESIAN_POINT ( 'NONE',  ( 7.288334046976859604, 4.602115691088532579, 21.08258158336541399 ) ) ;
#7099 = UNCERTAINTY_MEASURE_WITH_UNIT (LENGTH_MEASURE( 1.000000000000000082E-05 ), #3610, 'distance_accuracy_value', 'NONE');
#7100 = ORIENTED_EDGE ( 'NONE', *, *, #10931, .F. ) ;
#7102 = ORIENTED_EDGE ( 'NONE', *, *, #12455, .F. ) ;
#7101 = DIRECTION ( 'NONE',  ( 0.8719950447285833572, 0.4895147004624025300, 4.067366430758019417E-16 ) ) ;
#7103 = VERTEX_POINT ( 'NONE', #2688 ) ;
#7104 = FACE_OUTER_BOUND ( 'NONE', #12660, .T. ) ;
#7105 = ORIENTED_EDGE ( 'NONE', *, *, #10701, .T. ) ;
#7106 = CARTESIAN_POINT ( 'NONE',  ( 0.8003001391889992266, 20.99262100756200056, 16.16206422150100153 ) ) ;
#7107 = LINE ( 'NONE', #7188, #12100 ) ;
#7108 = VECTOR ( 'NONE', #9880, 1000.000000000000227 ) ;
#7109 = CARTESIAN_POINT ( 'NONE',  ( -10.22560374232860347, -19.62253721876480483, 56.85231026484400019 ) ) ;
#7110 = CARTESIAN_POINT ( 'NONE',  ( 0.000000000000000000, 0.000000000000000000, 0.000000000000000000 ) ) ;
#7111 = PLANE ( 'NONE',  #6044 ) ;
#7112 = LINE ( 'NONE', #5893, #13791 ) ;
#7113 = EDGE_CURVE ( 'NONE', #2114, #9929, #14318, .T. ) ;
#7114 = DIRECTION ( 'NONE',  ( 0.2975196656470014966, -0.9547156899063178326, 8.090169943749475688E-16 ) ) ;
#7115 = AXIS2_PLACEMENT_3D ( 'NONE', #14031, #3547, #11804 ) ;
#7116 = CARTESIAN_POINT ( 'NONE',  ( 5.799466111164440996, -37.30547240248169771, -11.36184443632733654 ) ) ;
#7117 = ORIENTED_EDGE ( 'NONE', *, *, #12080, .F. ) ;
#7118 = CARTESIAN_POINT ( 'NONE',  ( -15.49969986081099904, -13.50737899243800122, 6.712064221500998684 ) ) ;
#7119 = EDGE_LOOP ( 'NONE', ( #1111, #12334, #14606, #10133 ) ) ;
#7120 = ORIENTED_EDGE ( 'NONE', *, *, #10381, .F. ) ;
#7121 = VECTOR ( 'NONE', #9679, 1000.000000000000000 ) ;
#7122 = VECTOR ( 'NONE', #7398, 1000.000000000000000 ) ;
#7123 = PLANE ( 'NONE',  #7115 ) ;
#7124 = VERTEX_POINT ( 'NONE', #1541 ) ;
#7125 = CYLINDRICAL_SURFACE ( 'NONE', #6884, 2.499999999999998668 ) ;
#7126 = EDGE_CURVE ( 'NONE', #8808, #9099, #6265, .T. ) ;
#7127 = DIRECTION ( 'NONE',  ( -8.018662683283438208E-16, 5.975035461963189015E-16, 1.000000000000000000 ) ) ;
#7128 = VECTOR ( 'NONE', #13820, 1000.000000000000000 ) ;
#7129 = CARTESIAN_POINT ( 'NONE',  ( -13.26641246986315359, -91.82643169460182264, -10.39079603009238006 ) ) ;
#7130 = AXIS2_PLACEMENT_3D ( 'NONE', #4280, #8861, #14762 ) ;
#7131 =( BOUNDED_CURVE ( )  B_SPLINE_CURVE ( 3, ( #10687, #9539, #14208, #9391 ),
 .UNSPECIFIED., .F., .T. ) 
 B_SPLINE_CURVE_WITH_KNOTS ( ( 4, 4 ),
 ( 1.023945376098953641, 1.222940073837788466 ),
 .UNSPECIFIED. ) 
 CURVE ( )  GEOMETRIC_REPRESENTATION_ITEM ( )  RATIONAL_B_SPLINE_CURVE ( ( 1.000000000000000000, 0.9967028139718016044, 0.9967028139718016044, 1.000000000000000000 ) ) 
 REPRESENTATION_ITEM ( '' )  );
#7132 = VECTOR ( 'NONE', #11374, 1000.000000000000000 ) ;
#7133 = AXIS2_PLACEMENT_3D ( 'NONE', #7266, #336, #14325 ) ;
#7134 = CARTESIAN_POINT ( 'NONE',  ( -14.76203582817000282, -106.8625236479798843, -4.516005275576693734 ) ) ;
#7136 = DIRECTION ( 'NONE',  ( 0.000000000000000000, 0.000000000000000000, 1.000000000000000000 ) ) ;
#7135 = FACE_OUTER_BOUND ( 'NONE', #14625, .T. ) ;
#7137 = ORIENTED_EDGE ( 'NONE', *, *, #11650, .T. ) ;
#7138 = DIRECTION ( 'NONE',  ( 1.000000000000000000, 1.000000000000000078E-15, 1.000000000000000078E-15 ) ) ;
#7139 = CARTESIAN_POINT ( 'NONE',  ( -14.99866629829804765, -4.445910272123860807, 57.00231026484397745 ) ) ;
#7140 = ORIENTED_EDGE ( 'NONE', *, *, #8228, .F. ) ;
#7141 = ORIENTED_EDGE ( 'NONE', *, *, #4571, .T. ) ;
#7142 = CARTESIAN_POINT ( 'NONE',  ( -21.86069005650799468, -39.62793443228212453, 56.46004693087562032 ) ) ;
#7143 = ORIENTED_EDGE ( 'NONE', *, *, #3539, .T. ) ;
#7144 = SURFACE_STYLE_USAGE ( .BOTH. , #2490 ) ;
#7145 = CIRCLE ( 'NONE', #7623, 4.500000000000000000 ) ;
#7146 = ADVANCED_FACE ( 'NONE', ( #6192 ), #402, .T. ) ;
#7147 = CARTESIAN_POINT ( 'NONE',  ( -15.49969986081099727, 71.39262100756199914, 32.52626782222684909 ) ) ;
#7148 = DIRECTION ( 'NONE',  ( -1.000000000000000000, -1.201369187114119994E-15, -9.616040805000176517E-16 ) ) ;
#7149 = AXIS2_PLACEMENT_3D ( 'NONE', #9899, #3011, #14792 ) ;
#7150 = AXIS2_PLACEMENT_3D ( 'NONE', #2601, #2677, #10632 ) ;
#7151 = CARTESIAN_POINT ( 'NONE',  ( -15.49969986081092088, -13.50737899243822504, 56.85231026484398598 ) ) ;
#7152 = CARTESIAN_POINT ( 'NONE',  ( -23.49969986081099904, -19.50737899243800300, 60.84879442494580104 ) ) ;
#7153 = ORIENTED_EDGE ( 'NONE', *, *, #10510, .T. ) ;
#7154 = CIRCLE ( 'NONE', #7647, 2.458500000000002572 ) ;
#7155 = LINE ( 'NONE', #4886, #13382 ) ;
#7156 = CIRCLE ( 'NONE', #581, 22.99999999999999645 ) ;
#7157 = DIRECTION ( 'NONE',  ( 0.5975035461963188466, 0.8018662683283437342, 0.000000000000000000 ) ) ;
#7158 = ORIENTED_EDGE ( 'NONE', *, *, #9159, .T. ) ;
#7159 = DIRECTION ( 'NONE',  ( 0.5975035461963189576, 0.8018662683283437342, 0.000000000000000000 ) ) ;
#7160 = VERTEX_POINT ( 'NONE', #11016 ) ;
#7161 = CARTESIAN_POINT ( 'NONE',  ( -17.62015867087677634, -21.29935591968936137, 56.85231026484400019 ) ) ;
#7162 = ORIENTED_EDGE ( 'NONE', *, *, #7570, .F. ) ;
#7163 = CARTESIAN_POINT ( 'NONE',  ( -7.707227416580196611, -8.855645637450560770, 56.85231026484400019 ) ) ;
#7164 = LINE ( 'NONE', #1286, #11926 ) ;
#7165 = CARTESIAN_POINT ( 'NONE',  ( -8.701256315749452241, -15.46758698257906950, 57.00231026484399166 ) ) ;
#7166 = AXIS2_PLACEMENT_3D ( 'NONE', #13231, #5039, #2737 ) ;
#7167 = ADVANCED_FACE ( 'NONE', ( #4991 ), #8716, .T. ) ;
#7168 = PLANE ( 'NONE',  #13014 ) ;
#7169 = CARTESIAN_POINT ( 'NONE',  ( -3.508527451664997798, -48.23942980000687442, -5.497689735155999458 ) ) ;
#7170 = EDGE_CURVE ( 'NONE', #6540, #15034, #9650, .T. ) ;
#7171 = CARTESIAN_POINT ( 'NONE',  ( -18.61476135779618346, -20.95734656753543845, 56.85231026484398598 ) ) ;
#7172 = VECTOR ( 'NONE', #12692, 1000.000000000000227 ) ;
#7173 = CARTESIAN_POINT ( 'NONE',  ( 18.53245405280430802, -27.00737899243800300, 8.462064221501000461 ) ) ;
#7174 = DIRECTION ( 'NONE',  ( 0.000000000000000000, 0.000000000000000000, 1.000000000000000000 ) ) ;
#7175 = CARTESIAN_POINT ( 'NONE',  ( -20.87112600995946110, -108.1670994135940020, -5.659551793623918137 ) ) ;
#7176 = CIRCLE ( 'NONE', #2794, 2.499999999999998668 ) ;
#7177 = PLANE ( 'NONE',  #12800 ) ;
#7178 = ORIENTED_EDGE ( 'NONE', *, *, #14109, .F. ) ;
#7179 = DIRECTION ( 'NONE',  ( 8.018662683283438208E-16, -5.975035461963189015E-16, -1.000000000000000000 ) ) ;
#7180 = ORIENTED_EDGE ( 'NONE', *, *, #6504, .T. ) ;
#7182 = EDGE_LOOP ( 'NONE', ( #430, #15076, #13786, #10578 ) ) ;
#7181 = DIRECTION ( 'NONE',  ( -1.000000000000000000, -1.201369187114119994E-15, -9.616040805000176517E-16 ) ) ;
#7183 = ORIENTED_EDGE ( 'NONE', *, *, #10207, .T. ) ;
#7184 = DIRECTION ( 'NONE',  ( -1.000000000000000000, -1.201369187114119994E-15, -9.616040805000176517E-16 ) ) ;
#7185 = ORIENTED_EDGE ( 'NONE', *, *, #5208, .F. ) ;
#7186 = EDGE_CURVE ( 'NONE', #6669, #13555, #617, .T. ) ;
#7187 = EDGE_CURVE ( 'NONE', #4342, #1606, #4059, .T. ) ;
#7188 = CARTESIAN_POINT ( 'NONE',  ( -16.17213342976032209, -5.460076146431361188, 56.85231026484398598 ) ) ;
#7189 = VECTOR ( 'NONE', #13472, 1000.000000000000000 ) ;
#7190 = EDGE_CURVE ( 'NONE', #8640, #11007, #7436, .T. ) ;
#7191 = CARTESIAN_POINT ( 'NONE',  ( -16.24681173062539230, -5.467015265965240012, 57.00231026484397745 ) ) ;
#7192 = CARTESIAN_POINT ( 'NONE',  ( 5.898059818321144121E-14, -59.41623658196788682, 64.51922140836349229 ) ) ;
#7193 = DIRECTION ( 'NONE',  ( -8.018662683283438208E-16, 5.975035461963189015E-16, 1.000000000000000000 ) ) ;
#7194 = EDGE_CURVE ( 'NONE', #12515, #3791, #9797, .T. ) ;
#7195 = DIRECTION ( 'NONE',  ( 8.018662683283438208E-16, -5.975035461963189015E-16, -1.000000000000000000 ) ) ;
#7196 = CARTESIAN_POINT ( 'NONE',  ( 2.540007305964766093, -41.28381732925497971, -13.37362536790431022 ) ) ;
#7197 = VERTEX_POINT ( 'NONE', #11948 ) ;
#7198 = EDGE_LOOP ( 'NONE', ( #12562, #3697, #6187, #12752 ) ) ;
#7199 = ORIENTED_EDGE ( 'NONE', *, *, #1524, .F. ) ;
#7200 = AXIS2_PLACEMENT_3D ( 'NONE', #9549, #12936, #2444 ) ;
#7201 = DIRECTION ( 'NONE',  ( -0.9966498018049937402, 0.08178736187251965661, -8.480480961564258050E-16 ) ) ;
#7202 = VERTEX_POINT ( 'NONE', #1465 ) ;
#7203 = PLANE ( 'NONE',  #3455 ) ;
#7204 = FACE_OUTER_BOUND ( 'NONE', #2268, .T. ) ;
#7205 = ADVANCED_FACE ( 'NONE', ( #10798 ), #328, .F. ) ;
#7206 = EDGE_CURVE ( 'NONE', #2844, #1400, #12321, .T. ) ;
#7207 = ADVANCED_FACE ( 'NONE', ( #3135 ), #6483, .T. ) ;
#7208 = CARTESIAN_POINT ( 'NONE',  ( -14.84437367148764686, -93.78075803281299727, -10.82899037021154953 ) ) ;
#7209 = DIRECTION ( 'NONE',  ( 0.000000000000000000, -1.000000000000000000, -1.224646799147350002E-16 ) ) ;
#7211 = CARTESIAN_POINT ( 'NONE',  ( -38.49826176900612751, 3.992621007561997892, 24.89858491813232177 ) ) ;
#7210 = CARTESIAN_POINT ( 'NONE',  ( -7.499706911750001481, -49.00740941973812426, -5.271278242526713953 ) ) ;
#7212 = ORIENTED_EDGE ( 'NONE', *, *, #302, .T. ) ;
#7213 = LINE ( 'NONE', #11893, #4098 ) ;
#7214 = CARTESIAN_POINT ( 'NONE',  ( -23.82178639965737688, -19.07793027397611141, 60.77846357673786315 ) ) ;
#7215 = ORIENTED_EDGE ( 'NONE', *, *, #13526, .F. ) ;
#7216 = ORIENTED_EDGE ( 'NONE', *, *, #6536, .F. ) ;
#7217 = EDGE_CURVE ( 'NONE', #6762, #5844, #10087, .T. ) ;
#7218 = CARTESIAN_POINT ( 'NONE',  ( -23.07797347600723015, -41.93085761288553215, 56.22867446278029036 ) ) ;
#7219 = ORIENTED_EDGE ( 'NONE', *, *, #93, .T. ) ;
#7220 = CARTESIAN_POINT ( 'NONE',  ( -18.41596830400278506, -14.76384693893611910, 57.00231026484397745 ) ) ;
#7221 =( BOUNDED_CURVE ( )  B_SPLINE_CURVE ( 3, ( #9049, #8973, #1099, #11503 ),
 .UNSPECIFIED., .F., .T. ) 
 B_SPLINE_CURVE_WITH_KNOTS ( ( 4, 4 ),
 ( 6.505213034913054214E-16, 1.513547814233603184 ),
 .UNSPECIFIED. ) 
 CURVE ( )  GEOMETRIC_REPRESENTATION_ITEM ( )  RATIONAL_B_SPLINE_CURVE ( ( 1.000000000000000000, 0.8180365063541295001, 0.8180365063541295001, 1.000000000000000000 ) ) 
 REPRESENTATION_ITEM ( '' )  );
#7222 = AXIS2_PLACEMENT_3D ( 'NONE', #903, #14526, #8701 ) ;
#7223 = LINE ( 'NONE', #1575, #13437 ) ;
#7224 = CARTESIAN_POINT ( 'NONE',  ( -7.016473591028805856, -8.259951331604915126, 54.00231026484399166 ) ) ;
#7225 = CARTESIAN_POINT ( 'NONE',  ( -7.541204214081353108, -45.30969539143143976, 17.30566581272957905 ) ) ;
#7226 = DIRECTION ( 'NONE',  ( 8.018662683283438208E-16, -5.975035461963189015E-16, -1.000000000000000000 ) ) ;
#7227 = VERTEX_POINT ( 'NONE', #8940 ) ;
#7228 = CARTESIAN_POINT ( 'NONE',  ( -15.49969986081092088, -13.50737899243822504, 56.85231026484398598 ) ) ;
#7229 = VERTEX_POINT ( 'NONE', #8867 ) ;
#7230 = EDGE_CURVE ( 'NONE', #777, #5522, #11392, .T. ) ;
#7231 = CARTESIAN_POINT ( 'NONE',  ( -7.512805849530849400, -44.04964101872670312, 19.04457229113268113 ) ) ;
#7232 = ORIENTED_EDGE ( 'NONE', *, *, #11063, .T. ) ;
#7233 = DIRECTION ( 'NONE',  ( 8.018662683283438208E-16, -5.975035461963189015E-16, -1.000000000000000000 ) ) ;
#7234 = ORIENTED_EDGE ( 'NONE', *, *, #7732, .F. ) ;
#7235 = STYLED_ITEM ( 'NONE', ( #1551 ), #2515 ) ;
#7236 = DIRECTION ( 'NONE',  ( 0.000000000000000000, 0.1872998510044759646, 0.9823027872370621028 ) ) ;
#7237 = CARTESIAN_POINT ( 'NONE',  ( -17.05536012119625866, -6.605120582739408164, 56.85231026484398598 ) ) ;
#7238 = CARTESIAN_POINT ( 'NONE',  ( -7.758527451664999575, -46.50737899243799944, -5.497689735156000346 ) ) ;
#7239 = AXIS2_PLACEMENT_3D ( 'NONE', #7571, #6416, #13181 ) ;
#7240 = DIRECTION ( 'NONE',  ( 0.3633925226508256667, -0.9316361277244830097, 8.480480961564259036E-16 ) ) ;
#7241 = VECTOR ( 'NONE', #8544, 1000.000000000000000 ) ;
#7242 = CARTESIAN_POINT ( 'NONE',  ( -7.506093261461533217, -14.65346081099997910, 57.00231026484399166 ) ) ;
#7243 = ORIENTED_EDGE ( 'NONE', *, *, #214, .T. ) ;
#7244 = DIRECTION ( 'NONE',  ( 0.000000000000000000, 0.000000000000000000, 1.000000000000000000 ) ) ;
#7245 = CARTESIAN_POINT ( 'NONE',  ( -34.11203994331643230, -39.60748137432106830, 52.05738518461070896 ) ) ;
#7246 = DIRECTION ( 'NONE',  ( -0.9997391571607663341, -0.02283895005206026604, -7.880107536067206944E-16 ) ) ;
#7247 = EDGE_CURVE ( 'NONE', #6704, #951, #13547, .T. ) ;
#7248 = ORIENTED_EDGE ( 'NONE', *, *, #2353, .T. ) ;
#7249 = DIRECTION ( 'NONE',  ( 8.018662683283438208E-16, -5.975035461963189015E-16, -1.000000000000000000 ) ) ;
#7250 = VERTEX_POINT ( 'NONE', #4365 ) ;
#7251 = CIRCLE ( 'NONE', #11175, 3.000000000000002665 ) ;
#7253 = ORIENTED_EDGE ( 'NONE', *, *, #8116, .F. ) ;
#7252 = DIRECTION ( 'NONE',  ( 0.000000000000000000, 0.1872998510044689147, 0.9823027872370635460 ) ) ;
#7254 = VERTEX_POINT ( 'NONE', #6788 ) ;
#7255 = EDGE_CURVE ( 'NONE', #11739, #5451, #12474, .T. ) ;
#7256 = CIRCLE ( 'NONE', #205, 23.00000000000000000 ) ;
#7257 = LINE ( 'NONE', #9934, #12521 ) ;
#7258 = ORIENTED_EDGE ( 'NONE', *, *, #14769, .T. ) ;
#7259 = DIRECTION ( 'NONE',  ( -8.018662683283438208E-16, 5.975035461963189015E-16, 1.000000000000000000 ) ) ;
#7260 = DIRECTION ( 'NONE',  ( 0.9826409426582659590, -0.1855175943453191700, 8.987940462991681405E-16 ) ) ;
#7261 = DIRECTION ( 'NONE',  ( -8.018662683283438208E-16, 5.975035461963189015E-16, 1.000000000000000000 ) ) ;
#7262 = AXIS2_PLACEMENT_3D ( 'NONE', #14492, #4012, #1566 ) ;
#7263 = CARTESIAN_POINT ( 'NONE',  ( -15.49969986081092088, -13.50737899243822504, 56.85231026484398598 ) ) ;
#7264 = CIRCLE ( 'NONE', #3866, 9.974999999999999645 ) ;
#7265 = VECTOR ( 'NONE', #3256, 1000.000000000000114 ) ;
#7266 = CARTESIAN_POINT ( 'NONE',  ( -15.49969986081091022, -13.50737899243823215, 45.50231026484398456 ) ) ;
#7267 = ADVANCED_FACE ( 'NONE', ( #6636 ), #14767, .T. ) ;
#7268 = CARTESIAN_POINT ( 'NONE',  ( 4.269688099973369511, -38.19079675818824882, -12.36340031411550733 ) ) ;
#7269 = EDGE_CURVE ( 'NONE', #1866, #5883, #2069, .T. ) ;
#7270 = ORIENTED_EDGE ( 'NONE', *, *, #10466, .F. ) ;
#7271 = DIRECTION ( 'NONE',  ( 0.9472588896649092316, -0.3204693369899889732, 9.510565162951523791E-16 ) ) ;
#7272 = DIRECTION ( 'NONE',  ( 1.000000000000000000, 1.201369187114119994E-15, 9.616040805000176517E-16 ) ) ;
#7273 = ORIENTED_EDGE ( 'NONE', *, *, #9140, .T. ) ;
#7274 = ORIENTED_EDGE ( 'NONE', *, *, #11266, .F. ) ;
#7275 = LINE ( 'NONE', #114, #1761 ) ;
#7276 = EDGE_CURVE ( 'NONE', #10198, #11004, #7677, .T. ) ;
#7277 = CARTESIAN_POINT ( 'NONE',  ( -1.508527451664997354, -48.96587899243800024, -5.497689735156000346 ) ) ;
#7278 = ORIENTED_EDGE ( 'NONE', *, *, #454, .T. ) ;
#7279 = VECTOR ( 'NONE', #1993, 1000.000000000000000 ) ;
#7280 = LINE ( 'NONE', #6916, #5158 ) ;
#7281 = CARTESIAN_POINT ( 'NONE',  ( -16.58746603607633929, -23.42289157363887142, 54.00231026484399166 ) ) ;
#7282 = EDGE_CURVE ( 'NONE', #5816, #2807, #13009, .T. ) ;
#7283 = CARTESIAN_POINT ( 'NONE',  ( -17.98267069058175593, -13.21607870320540457, 51.00231026484399166 ) ) ;
#7284 = CARTESIAN_POINT ( 'NONE',  ( -9.376966593418606166, -18.77214511605354019, 56.85231026484400019 ) ) ;
#7285 = MANIFOLD_SOLID_BREP ( 'Stock-MAS-672-1', #8277 ) ;
#7286 = AXIS2_PLACEMENT_3D ( 'NONE', #10663, #8361, #9590 ) ;
#7287 = CARTESIAN_POINT ( 'NONE',  ( -15.49969986081099904, 64.39262100756199914, 24.21206422150100579 ) ) ;
#7289 = CARTESIAN_POINT ( 'NONE',  ( -15.49969986081099904, 12.99262100756199878, 24.21206422150099868 ) ) ;
#7288 = CARTESIAN_POINT ( 'NONE',  ( -7.607412389351755344, -48.63717025145610506, -6.846874655572149138 ) ) ;
#7290 = EDGE_CURVE ( 'NONE', #4715, #10921, #12704, .T. ) ;
#7291 = VECTOR ( 'NONE', #9443, 1000.000000000000000 ) ;
#7292 = ORIENTED_EDGE ( 'NONE', *, *, #15055, .F. ) ;
#7293 = DIRECTION ( 'NONE',  ( -8.018662683283438208E-16, 5.975035461963189015E-16, 1.000000000000000000 ) ) ;
#7294 = EDGE_CURVE ( 'NONE', #12315, #7352, #10625, .T. ) ;
#7295 = CARTESIAN_POINT ( 'NONE',  ( -25.28633754730619643, -15.63094115750824820, 60.41261054227882710 ) ) ;
#7296 = EDGE_LOOP ( 'NONE', ( #13285, #8429, #9258, #7523 ) ) ;
#7297 = ORIENTED_EDGE ( 'NONE', *, *, #12542, .F. ) ;
#7298 = CARTESIAN_POINT ( 'NONE',  ( 21.88653531229833860, -28.45002520398911727, 27.13200563053409553 ) ) ;
#7299 = CARTESIAN_POINT ( 'NONE',  ( -1.508527451664997798, -47.80641709811465034, -4.747689735156000346 ) ) ;
#7300 = VERTEX_POINT ( 'NONE', #4899 ) ;
#7301 = CONICAL_SURFACE ( 'NONE', #6561, 6.250000000000001776, 0.7853981633974461696 ) ;
#7302 = CARTESIAN_POINT ( 'NONE',  ( -12.84086554789186607, -5.882298658668338120, 57.00231026484397745 ) ) ;
#7303 = AXIS2_PLACEMENT_3D ( 'NONE', #9345, #14016, #3534 ) ;
#7304 = DIRECTION ( 'NONE',  ( 0.000000000000000000, -1.850371707708594563E-16, 1.000000000000000000 ) ) ;
#7305 = CARTESIAN_POINT ( 'NONE',  ( -9.919921220328577149, -21.80813450786784102, 56.58478691063636035 ) ) ;
#7306 = VECTOR ( 'NONE', #3038, 1000.000000000000000 ) ;
#7307 = LINE ( 'NONE', #6081, #8930 ) ;
#7308 = DIRECTION ( 'NONE',  ( 0.9918751611018171710, 0.1272150336605075427, 7.193398003386516820E-16 ) ) ;
#7309 = ORIENTED_EDGE ( 'NONE', *, *, #2384, .F. ) ;
#7310 = DIRECTION ( 'NONE',  ( -1.011922027653136551E-15, 1.000000000000000000, 0.000000000000000000 ) ) ;
#7311 = CARTESIAN_POINT ( 'NONE',  ( -11.55238169831532957, -21.67927775123549594, 56.85231026484400019 ) ) ;
#7312 = VERTEX_POINT ( 'NONE', #3362 ) ;
#7313 = ADVANCED_FACE ( 'NONE', ( #13921 ), #5727, .F. ) ;
#7314 = FACE_OUTER_BOUND ( 'NONE', #1869, .T. ) ;
#7315 = CARTESIAN_POINT ( 'NONE',  ( -15.49969986081092088, -13.50737899243822504, 57.00231026484397745 ) ) ;
#7316 = ORIENTED_EDGE ( 'NONE', *, *, #7294, .F. ) ;
#7317 =( BOUNDED_CURVE ( )  B_SPLINE_CURVE ( 3, ( #13183, #1320, #5975, #176 ),
 .UNSPECIFIED., .F., .F. ) 
 B_SPLINE_CURVE_WITH_KNOTS ( ( 4, 4 ),
 ( -8.881784197001252323E-16, 1.570796326794907216 ),
 .UNSPECIFIED. ) 
 CURVE ( )  GEOMETRIC_REPRESENTATION_ITEM ( )  RATIONAL_B_SPLINE_CURVE ( ( 1.000000000000000000, 0.8047378541243622729, 0.8047378541243622729, 1.000000000000000000 ) ) 
 REPRESENTATION_ITEM ( '' )  );
#7318 = CARTESIAN_POINT ( 'NONE',  ( -7.497874475122997318, -44.50608669435617770, -6.993290823733421036 ) ) ;
#7319 = VERTEX_POINT ( 'NONE', #9551 ) ;
#7320 = CARTESIAN_POINT ( 'NONE',  ( -7.499699860810999041, -19.50737899243799589, 56.13904046828879757 ) ) ;
#7321 = DIRECTION ( 'NONE',  ( -0.8018662683283436232, 0.5975035461963189576, -9.999999999999996833E-16 ) ) ;
#7322 = EDGE_CURVE ( 'NONE', #14421, #2329, #11693, .T. ) ;
#7323 = EDGE_CURVE ( 'NONE', #5828, #2471, #4741, .T. ) ;
#7324 = CARTESIAN_POINT ( 'NONE',  ( -7.821533452793039132, -47.59505538333821306, 17.25098663457825410 ) ) ;
#7325 = AXIS2_PLACEMENT_3D ( 'NONE', #8283, #268, #2558 ) ;
#7326 = CARTESIAN_POINT ( 'NONE',  ( 18.10049798887294514, -29.26525578417205153, 7.559493535731737879 ) ) ;
#7327 = ORIENTED_EDGE ( 'NONE', *, *, #14773, .T. ) ;
#7328 = DIRECTION ( 'NONE',  ( 1.000000000000000000, 0.000000000000000000, 0.000000000000000000 ) ) ;
#7329 = DIRECTION ( 'NONE',  ( 0.000000000000000000, 0.1872998510044759646, 0.9823027872370621028 ) ) ;
#7330 = PRODUCT ( 'Dial Adjustment Screw', 'Dial Adjustment Screw', '', ( #4347 ) ) ;
#7331 = LINE ( 'NONE', #11936, #9108 ) ;
#7332 = ORIENTED_EDGE ( 'NONE', *, *, #6320, .F. ) ;
#7333 = CARTESIAN_POINT ( 'NONE',  ( -7.753733168396166775, -46.50737899243799944, 42.00231026484399166 ) ) ;
#7334 = ORIENTED_EDGE ( 'NONE', *, *, #8594, .T. ) ;
#7336 = ORIENTED_EDGE ( 'NONE', *, *, #4675, .F. ) ;
#7335 = DIRECTION ( 'NONE',  ( -8.018662683283438208E-16, 5.975035461963189015E-16, 1.000000000000000000 ) ) ;
#7337 = ORIENTED_EDGE ( 'NONE', *, *, #3740, .F. ) ;
#7338 = VECTOR ( 'NONE', #1088, 999.9999999999998863 ) ;
#7339 = FACE_OUTER_BOUND ( 'NONE', #8599, .T. ) ;
#7340 = ORIENTED_EDGE ( 'NONE', *, *, #9594, .T. ) ;
#7341 = FACE_OUTER_BOUND ( 'NONE', #8224, .T. ) ;
#7342 = EDGE_CURVE ( 'NONE', #6753, #1019, #10452, .T. ) ;
#7343 = CARTESIAN_POINT ( 'NONE',  ( -2.216578225681298697, -32.00737899243799944, 59.28069236156870403 ) ) ;
#7344 = APPLICATION_PROTOCOL_DEFINITION ( 'draft international standard', 'automotive_design', 1998, #13204 ) ;
#7345 = DIRECTION ( 'NONE',  ( 8.018662683283438208E-16, -5.975035461963189015E-16, -1.000000000000000000 ) ) ;
#7346 = LINE ( 'NONE', #4920, #13276 ) ;
#7347 = DIRECTION ( 'NONE',  ( -0.1511109077013150781, -0.9885168150181790070, 4.694715627858902218E-16 ) ) ;
#7348 = ORIENTED_EDGE ( 'NONE', *, *, #5503, .T. ) ;
#7349 = FACE_OUTER_BOUND ( 'NONE', #4047, .T. ) ;
#7350 = SURFACE_STYLE_FILL_AREA ( #10808 ) ;
#7351 = ORIENTED_EDGE ( 'NONE', *, *, #4560, .F. ) ;
#7352 = VERTEX_POINT ( 'NONE', #6862 ) ;
#7353 = CARTESIAN_POINT ( 'NONE',  ( -15.49969986081099904, -57.00737899243800655, 19.50231026484399877 ) ) ;
#7354 = EDGE_LOOP ( 'NONE', ( #12001, #8657, #7412, #14515, #4271, #5177 ) ) ;
#7355 = VERTEX_POINT ( 'NONE', #8169 ) ;
#7356 = VECTOR ( 'NONE', #3077, 1000.000000000000000 ) ;
#7357 = DIRECTION ( 'NONE',  ( 0.000000000000000000, -1.000000000000000000, -1.224646799147350002E-16 ) ) ;
#7358 = EDGE_CURVE ( 'NONE', #15087, #8216, #8172, .T. ) ;
#7359 = FACE_OUTER_BOUND ( 'NONE', #592, .T. ) ;
#7360 = EDGE_CURVE ( 'NONE', #10290, #11428, #3589, .T. ) ;
#7361 = AXIS2_PLACEMENT_3D ( 'NONE', #9758, #1717, #6369 ) ;
#7362 = AXIS2_PLACEMENT_3D ( 'NONE', #12793, #13928, #1226 ) ;
#7363 = DIRECTION ( 'NONE',  ( -1.000000000000000000, 0.000000000000000000, -9.688619527525975741E-16 ) ) ;
#7365 = FACE_OUTER_BOUND ( 'NONE', #14140, .T. ) ;
#7364 = PLANE ( 'NONE',  #9313 ) ;
#7366 = ORIENTED_EDGE ( 'NONE', *, *, #14320, .T. ) ;
#7367 = CARTESIAN_POINT ( 'NONE',  ( -20.18599136182624676, -52.50737899243804208, 11.50231026484396502 ) ) ;
#7368 = ORIENTED_EDGE ( 'NONE', *, *, #2626, .T. ) ;
#7369 = CARTESIAN_POINT ( 'NONE',  ( -14.84437367148764686, -93.78075803281299727, -10.82899037021154953 ) ) ;
#7370 = ORIENTED_EDGE ( 'NONE', *, *, #1334, .T. ) ;
#7371 = ORIENTED_EDGE ( 'NONE', *, *, #9357, .T. ) ;
#7372 = CARTESIAN_POINT ( 'NONE',  ( -18.08681813700378171, -52.08207165106512093, 56.91381011686954849 ) ) ;
#7373 = VERTEX_POINT ( 'NONE', #5949 ) ;
#7374 = EDGE_CURVE ( 'NONE', #5152, #5621, #3872, .T. ) ;
#7375 = VECTOR ( 'NONE', #10690, 1000.000000000000227 ) ;
#7376 = AXIS2_PLACEMENT_3D ( 'NONE', #13763, #10010, #915 ) ;
#7377 = VECTOR ( 'NONE', #7687, 1000.000000000000227 ) ;
#7378 = VECTOR ( 'NONE', #4283, 1000.000000000000000 ) ;
#7379 = ADVANCED_FACE ( 'NONE', ( #7529, #7749 ), #8905, .T. ) ;
#7380 = CYLINDRICAL_SURFACE ( 'NONE', #12205, 37.49999999999999289 ) ;
#7381 = EDGE_CURVE ( 'NONE', #1870, #2152, #9906, .T. ) ;
#7382 = CARTESIAN_POINT ( 'NONE',  ( -23.12048770254168062, -16.17743848078839619, 57.00231026484397745 ) ) ;
#7383 = EDGE_CURVE ( 'NONE', #6584, #1349, #1805, .T. ) ;
#7384 = FACE_OUTER_BOUND ( 'NONE', #5942, .T. ) ;
#7385 = CYLINDRICAL_SURFACE ( 'NONE', #3007, 0.4500000000000011768 ) ;
#7386 = ORIENTED_EDGE ( 'NONE', *, *, #2316, .T. ) ;
#7387 = CARTESIAN_POINT ( 'NONE',  ( -9.508527451664999575, -46.50737899243799944, -5.497689735156000346 ) ) ;
#7388 = AXIS2_PLACEMENT_3D ( 'NONE', #2177, #3322, #4547 ) ;
#7389 = FACE_OUTER_BOUND ( 'NONE', #12425, .T. ) ;
#7390 = ORIENTED_EDGE ( 'NONE', *, *, #6521, .T. ) ;
#7391 = AXIS2_PLACEMENT_3D ( 'NONE', #2150, #7945, #4597 ) ;
#7392 = CARTESIAN_POINT ( 'NONE',  ( -18.09969986081100402, -102.1080954886104877, -6.186719399335088632 ) ) ;
#7393 =( LENGTH_UNIT ( ) NAMED_UNIT ( * ) SI_UNIT ( .MILLI., .METRE. ) );
#7394 = VERTEX_POINT ( 'NONE', #13584 ) ;
#7395 = LINE ( 'NONE', #11073, #8144 ) ;
#7396 = ORIENTED_EDGE ( 'NONE', *, *, #38, .T. ) ;
#7397 = CARTESIAN_POINT ( 'NONE',  ( -22.56723502526082470, -13.84084068328822248, 56.85231026484398598 ) ) ;
#7398 = DIRECTION ( 'NONE',  ( 1.000000000000000000, 1.201369187114119994E-15, 9.616040805000176517E-16 ) ) ;
#7399 = ADVANCED_FACE ( 'NONE', ( #5463 ), #4761, .T. ) ;
#7400 = CIRCLE ( 'NONE', #819, 4.500000000000000000 ) ;
#7401 = AXIS2_PLACEMENT_3D ( 'NONE', #4833, #7181, #7252 ) ;
#7402 = CARTESIAN_POINT ( 'NONE',  ( -7.501378586840248275, -49.00244658604240300, 19.34197447739098763 ) ) ;
#7403 = AXIS2_PLACEMENT_3D ( 'NONE', #12213, #4330, #7683 ) ;
#7404 = CARTESIAN_POINT ( 'NONE',  ( 16.32110505353168861, -30.15237131756928690, 4.369237647224089471 ) ) ;
#7405 = LINE ( 'NONE', #105, #13060 ) ;
#7406 = EDGE_LOOP ( 'NONE', ( #2462, #3974 ) ) ;
#7407 = LINE ( 'NONE', #2449, #5781 ) ;
#7408 = CARTESIAN_POINT ( 'NONE',  ( -15.57469986081099478, -23.50709773848280904, 56.85231026484400019 ) ) ;
#7409 = CARTESIAN_POINT ( 'NONE',  ( -7.505475668120653587, -44.32813276070414332, -4.257828788660135366 ) ) ;
#7410 = ORIENTED_EDGE ( 'NONE', *, *, #11266, .T. ) ;
#7412 = ORIENTED_EDGE ( 'NONE', *, *, #11504, .T. ) ;
#7411 = CARTESIAN_POINT ( 'NONE',  ( -33.59815531783383591, -41.01804242337339446, -13.34120349808900130 ) ) ;
#7413 = VERTEX_POINT ( 'NONE', #14576 ) ;
#7414 = ADVANCED_FACE ( 'NONE', ( #14223 ), #10983, .F. ) ;
#7415 = VECTOR ( 'NONE', #2440, 1000.000000000000114 ) ;
#7416 = DIRECTION ( 'NONE',  ( 0.4274949678123838859, -0.9040177279761104634, 8.829475928589268008E-16 ) ) ;
#7417 = DIRECTION ( 'NONE',  ( -0.4274949678123838859, 0.9040177279761104634, -8.829475928589268008E-16 ) ) ;
#7418 =( REPRESENTATION_RELATIONSHIP ('NONE','NONE', #2372, #10770 ) REPRESENTATION_RELATIONSHIP_WITH_TRANSFORMATION ( #2277 )SHAPE_REPRESENTATION_RELATIONSHIP( ) );
#7419 = CARTESIAN_POINT ( 'NONE',  ( -32.76014075162859740, 10.68321993080349763, 16.26994987741149856 ) ) ;
#7420 = VECTOR ( 'NONE', #13809, 1000.000000000000000 ) ;
#7421 = CARTESIAN_POINT ( 'NONE',  ( -7.795104587452824418, -46.66314860471634773, -2.997690171028501549 ) ) ;
#7422 = CARTESIAN_POINT ( 'NONE',  ( 16.50882759085405027, -70.29616524101228947, 42.07940533022636487 ) ) ;
#7423 = CARTESIAN_POINT ( 'NONE',  ( -15.49969986081099904, 70.89785811302749607, 24.21206422150100579 ) ) ;
#7424 = AXIS2_PLACEMENT_3D ( 'NONE', #896, #8920, #3337 ) ;
#7425 = FACE_OUTER_BOUND ( 'NONE', #15124, .T. ) ;
#7426 = DIRECTION ( 'NONE',  ( -8.018662683283438208E-16, 5.975035461963189015E-16, 1.000000000000000000 ) ) ;
#7427 = VERTEX_POINT ( 'NONE', #14728 ) ;
#7428 = DIRECTION ( 'NONE',  ( -8.018662683283438208E-16, 5.975035461963189015E-16, 1.000000000000000000 ) ) ;
#7429 = VERTEX_POINT ( 'NONE', #8677 ) ;
#7430 = ORIENTED_EDGE ( 'NONE', *, *, #4732, .T. ) ;
#7431 = ADVANCED_FACE ( 'NONE', ( #2869 ), #3532, .T. ) ;
#7432 = CARTESIAN_POINT ( 'NONE',  ( -15.49969986081099727, -19.50737899243800300, 19.50231026484402008 ) ) ;
#7433 = ORIENTED_EDGE ( 'NONE', *, *, #3047, .F. ) ;
#7434 = EDGE_CURVE ( 'NONE', #14532, #14421, #13360, .T. ) ;
#7435 = CARTESIAN_POINT ( 'NONE',  ( -15.49969986081099371, -110.4767567321826078, -8.667385457847048613 ) ) ;
#7436 = CIRCLE ( 'NONE', #6693, 0.2000000000000012046 ) ;
#7437 = CARTESIAN_POINT ( 'NONE',  ( -15.49969986081099904, 22.99262100756200056, 24.21206422150099868 ) ) ;
#7438 = CARTESIAN_POINT ( 'NONE',  ( -9.959408463899002584, -21.80230492564002276, 57.00231026484399166 ) ) ;
#7439 = FACE_OUTER_BOUND ( 'NONE', #13029, .T. ) ;
#7440 = VECTOR ( 'NONE', #7260, 1000.000000000000114 ) ;
#7442 = CARTESIAN_POINT ( 'NONE',  ( -35.92581786978435332, 5.967462257416473292, 18.89919563306356665 ) ) ;
#7441 = CARTESIAN_POINT ( 'NONE',  ( -7.567013331128950249, -48.78395362562350357, -6.570480905340088995 ) ) ;
#7443 = ORIENTED_EDGE ( 'NONE', *, *, #7753, .T. ) ;
#7444 = LINE ( 'NONE', #1792, #10200 ) ;
#7445 = ORIENTED_EDGE ( 'NONE', *, *, #10569, .F. ) ;
#7446 = DIRECTION ( 'NONE',  ( 0.000000000000000000, 0.1872998510044689147, 0.9823027872370635460 ) ) ;
#7447 = VERTEX_POINT ( 'NONE', #1954 ) ;
#7448 = ORIENTED_EDGE ( 'NONE', *, *, #10846, .T. ) ;
#7449 = EDGE_CURVE ( 'NONE', #4500, #4715, #807, .T. ) ;
#7450 = FACE_OUTER_BOUND ( 'NONE', #3580, .T. ) ;
#7451 = VERTEX_POINT ( 'NONE', #6372 ) ;
#7452 = EDGE_CURVE ( 'NONE', #970, #3001, #14039, .T. ) ;
#7453 = CARTESIAN_POINT ( 'NONE',  ( 2.374542637206501272, 7.183219930803497633, 17.76912582958182085 ) ) ;
#7454 = DIRECTION ( 'NONE',  ( 0.8415927028326188886, -0.5401126942952620968, 9.975640502598240034E-16 ) ) ;
#7455 = CARTESIAN_POINT ( 'NONE',  ( -9.418794693332646517, -21.44679481879670391, 56.50578474138158924 ) ) ;
#7456 = EDGE_CURVE ( 'NONE', #5960, #12040, #4093, .T. ) ;
#7457 = FACE_BOUND ( 'NONE', #12182, .T. ) ;
#7458 = CARTESIAN_POINT ( 'NONE',  ( -23.05384319539488658, -10.65421522557165623, 57.00231026484397745 ) ) ;
#7459 = ORIENTED_EDGE ( 'NONE', *, *, #4879, .F. ) ;
#7460 = DIRECTION ( 'NONE',  ( -0.1165201156931293391, -0.9931883319083343320, 4.999999999999998416E-16 ) ) ;
#7461 = MANIFOLD_SOLID_BREP ( 'Stock-MAS-672-1', #8769 ) ;
#7462 = DIRECTION ( 'NONE',  ( -8.018662683283439195E-16, 5.975035461963190001E-16, 1.000000000000000000 ) ) ;
#7463 = EDGE_LOOP ( 'NONE', ( #7216, #13097, #13343, #13893 ) ) ;
#7464 = EDGE_CURVE ( 'NONE', #3375, #11878, #3472, .T. ) ;
#7466 = ADVANCED_FACE ( 'NONE', ( #4322, #12504 ), #3323, .T. ) ;
#7465 = CARTESIAN_POINT ( 'NONE',  ( 21.97317718429104616, -24.08580327976269331, 22.77252883434266550 ) ) ;
#7467 = EDGE_LOOP ( 'NONE', ( #9617, #14796, #14287, #2321 ) ) ;
#7468 = AXIS2_PLACEMENT_3D ( 'NONE', #3799, #13069, #4954 ) ;
#7469 = FACE_OUTER_BOUND ( 'NONE', #3844, .T. ) ;
#7470 = VERTEX_POINT ( 'NONE', #2253 ) ;
#7471 = CARTESIAN_POINT ( 'NONE',  ( -15.49969986081099904, 20.99262100756200056, 24.21206422150099868 ) ) ;
#7472 = ADVANCED_FACE ( 'NONE', ( #15099, #13657 ), #4627, .F. ) ;
#7473 = DIRECTION ( 'NONE',  ( -8.018662683283438208E-16, 5.975035461963189015E-16, 1.000000000000000000 ) ) ;
#7474 = EDGE_CURVE ( 'NONE', #11428, #4941, #3671, .T. ) ;
#7475 = CARTESIAN_POINT ( 'NONE',  ( -7.681929635180945404, -48.34577715838003087, 17.80744637252912455 ) ) ;
#7476 = CARTESIAN_POINT ( 'NONE',  ( 18.35413756676371122, -28.54901284085133639, 8.082023903208540361 ) ) ;
#7477 = DIRECTION ( 'NONE',  ( 0.000000000000000000, 0.000000000000000000, 1.000000000000000000 ) ) ;
#7478 = VERTEX_POINT ( 'NONE', #3254 ) ;
#7479 = CARTESIAN_POINT ( 'NONE',  ( -18.48721759179245439, -17.51671033407998479, -13.99768973515600301 ) ) ;
#7480 = CARTESIAN_POINT ( 'NONE',  ( -33.49969986081093509, -41.64411882290328748, 52.39987856403602962 ) ) ;
#7481 = EDGE_LOOP ( 'NONE', ( #6072, #1303 ) ) ;
#7482 = EDGE_CURVE ( 'NONE', #13156, #3424, #10431, .T. ) ;
#7483 = ADVANCED_FACE ( 'NONE', ( #11358 ), #881, .F. ) ;
#7484 = ORIENTED_EDGE ( 'NONE', *, *, #6093, .F. ) ;
#7486 = ORIENTED_EDGE ( 'NONE', *, *, #4492, .T. ) ;
#7485 = DIRECTION ( 'NONE',  ( 0.000000000000000000, 1.000000000000000000, 1.224646799147350002E-16 ) ) ;
#7487 = ORIENTED_EDGE ( 'NONE', *, *, #601, .T. ) ;
#7488 = CARTESIAN_POINT ( 'NONE',  ( -24.01584079503567182, -10.37104457333969876, 56.85231026484398598 ) ) ;
#7489 = FACE_OUTER_BOUND ( 'NONE', #10809, .T. ) ;
#7490 = CARTESIAN_POINT ( 'NONE',  ( -15.61203582816999713, -107.9994814593942607, -7.057848339359948042 ) ) ;
#7491 = AXIS2_PLACEMENT_3D ( 'NONE', #14026, #4392, #14870 ) ;
#7492 = PRODUCT_DEFINITION_SHAPE ( 'NONE', 'NONE',  #15133 ) ;
#7493 = CARTESIAN_POINT ( 'NONE',  ( -7.886584594865180264, -46.96511696614940234, -3.039951761444701361 ) ) ;
#7494 = AXIS2_PLACEMENT_3D ( 'NONE', #3426, #4576, #10386 ) ;
#7495 = PRODUCT_DEFINITION ( 'UNKNOWN', '', #7050, #4673 ) ;
#7496 = FACE_OUTER_BOUND ( 'NONE', #5490, .T. ) ;
#7497 = ADVANCED_FACE ( 'NONE', ( #10203 ), #10280, .T. ) ;
#7498 = DIRECTION ( 'NONE',  ( -1.000000000000000000, -1.000000000000000078E-15, 0.000000000000000000 ) ) ;
#7499 = AXIS2_PLACEMENT_3D ( 'NONE', #5172, #5326, #13366 ) ;
#7500 = FACE_BOUND ( 'NONE', #13559, .T. ) ;
#7501 = DIRECTION ( 'NONE',  ( 0.000000000000000000, -0.4999999999999993339, -0.8660254037844390407 ) ) ;
#7502 = ORIENTED_EDGE ( 'NONE', *, *, #7247, .F. ) ;
#7503 = CARTESIAN_POINT ( 'NONE',  ( -19.19431052208641120, -4.241825740657187538, 54.00231026484397745 ) ) ;
#7505 = ORIENTED_EDGE ( 'NONE', *, *, #11751, .T. ) ;
#7504 = CARTESIAN_POINT ( 'NONE',  ( -15.49969986081099904, -104.4958141456593097, -8.292482351415227271 ) ) ;
#7506 = VERTEX_POINT ( 'NONE', #13729 ) ;
#7507 = CARTESIAN_POINT ( 'NONE',  ( -15.61203582816999891, -108.0739289917895007, -5.561265332623595015 ) ) ;
#7508 = ORIENTED_EDGE ( 'NONE', *, *, #2141, .F. ) ;
#7509 = LINE ( 'NONE', #11189, #9511 ) ;
#7510 = AXIS2_PLACEMENT_3D ( 'NONE', #10785, #13320, #8558 ) ;
#7511 = AXIS2_PLACEMENT_3D ( 'NONE', #8368, #6975, #9675 ) ;
#7512 = FACE_OUTER_BOUND ( 'NONE', #9831, .T. ) ;
#7513 = VECTOR ( 'NONE', #3527, 1000.000000000000000 ) ;
#7514 = LINE ( 'NONE', #1859, #7528 ) ;
#7515 = ADVANCED_FACE ( 'NONE', ( #7973 ), #2180, .F. ) ;
#7516 = ADVANCED_FACE ( 'NONE', ( #6746 ), #9127, .F. ) ;
#7518 = CARTESIAN_POINT ( 'NONE',  ( -9.539601987502638991, -5.508762965862997518, 57.00231026484397745 ) ) ;
#7517 = DIRECTION ( 'NONE',  ( 8.018662683283438208E-16, -5.975035461963189015E-16, -1.000000000000000000 ) ) ;
#7519 = ORIENTED_EDGE ( 'NONE', *, *, #3916, .T. ) ;
#7520 = CARTESIAN_POINT ( 'NONE',  ( -15.49969986081092088, -13.50737899243822504, 57.00231026484397745 ) ) ;
#7521 = LINE ( 'NONE', #5155, #14827 ) ;
#7522 = ORIENTED_EDGE ( 'NONE', *, *, #6844, .T. ) ;
#7523 = ORIENTED_EDGE ( 'NONE', *, *, #2517, .T. ) ;
#7524 = VECTOR ( 'NONE', #14145, 1000.000000000000000 ) ;
#7525 = CARTESIAN_POINT ( 'NONE',  ( -25.43486656742121355, -12.61682438329676081, 57.00231026484397745 ) ) ;
#7526 = ORIENTED_EDGE ( 'NONE', *, *, #5026, .F. ) ;
#7527 = DIRECTION ( 'NONE',  ( 0.4800904676395346127, 0.8772189822852974883, -1.391731009600680140E-16 ) ) ;
#7528 = VECTOR ( 'NONE', #637, 1000.000000000000227 ) ;
#7529 = FACE_OUTER_BOUND ( 'NONE', #2546, .T. ) ;
#7530 = CARTESIAN_POINT ( 'NONE',  ( 5.426450521646303926, 12.65779542994540208, 32.26206422150099939 ) ) ;
#7531 = ADVANCED_FACE ( 'NONE', ( #4780 ), #14338, .T. ) ;
#7532 = CARTESIAN_POINT ( 'NONE',  ( -10.40142408276975594, -22.11861997768099641, 56.65522384219905661 ) ) ;
#7533 = CARTESIAN_POINT ( 'NONE',  ( -15.42469986081099442, -26.50737899243800300, 56.85231026484400019 ) ) ;
#7534 = DIRECTION ( 'NONE',  ( -0.5975035461963187355, -0.8018662683283439563, 0.000000000000000000 ) ) ;
#7535 = ORIENTED_EDGE ( 'NONE', *, *, #8914, .F. ) ;
#7536 = CARTESIAN_POINT ( 'NONE',  ( -18.06278547315525529, -11.75340479732393817, 57.00231026484397745 ) ) ;
#7537 = AXIS2_PLACEMENT_3D ( 'NONE', #4681, #10565, #6111 ) ;
#7538 = CARTESIAN_POINT ( 'NONE',  ( -15.12053853660593283, -5.441285657357897598, 56.85231026484398598 ) ) ;
#7539 = ORIENTED_EDGE ( 'NONE', *, *, #4961, .F. ) ;
#7540 = CARTESIAN_POINT ( 'NONE',  ( 21.85920135429434907, -27.00737899243800300, 20.96206422150100224 ) ) ;
#7541 = FACE_OUTER_BOUND ( 'NONE', #5529, .T. ) ;
#7542 = ORIENTED_EDGE ( 'NONE', *, *, #9704, .T. ) ;
#7543 = CARTESIAN_POINT ( 'NONE',  ( -20.33437667196779586, -7.039214636791314206, 56.85231026484398598 ) ) ;
#7544 = ORIENTED_EDGE ( 'NONE', *, *, #10660, .F. ) ;
#7545 = CARTESIAN_POINT ( 'NONE',  ( -8.858895634567668154, -20.95051974273374285, 54.00231026484400587 ) ) ;
#7546 = FACE_OUTER_BOUND ( 'NONE', #6048, .T. ) ;
#7547 = VECTOR ( 'NONE', #7357, 1000.000000000000000 ) ;
#7548 = AXIS2_PLACEMENT_3D ( 'NONE', #12917, #8300, #3797 ) ;
#7549 = EDGE_CURVE ( 'NONE', #5960, #2827, #13450, .T. ) ;
#7550 = DIRECTION ( 'NONE',  ( -0.8222303661035904598, 0.5691548339926102429, -9.993908270190959005E-16 ) ) ;
#7551 = DIRECTION ( 'NONE',  ( -0.7511640317997426708, -0.6601155939154560448, -2.079116908177589032E-16 ) ) ;
#7552 = CARTESIAN_POINT ( 'NONE',  ( 0.8003001391889992266, 20.99262100756200056, 24.21206422150100224 ) ) ;
#7553 = ADVANCED_FACE ( 'NONE', ( #14107 ), #8552, .F. ) ;
#7554 = EDGE_LOOP ( 'NONE', ( #8046, #10335, #5108, #763 ) ) ;
#7555 = CARTESIAN_POINT ( 'NONE',  ( -14.11952815701477881, -21.46390939632912875, 57.00231026484399166 ) ) ;
#7556 = LINE ( 'NONE', #236, #11924 ) ;
#7557 = ORIENTED_EDGE ( 'NONE', *, *, #12500, .T. ) ;
#7558 = VERTEX_POINT ( 'NONE', #2409 ) ;
#7560 = EDGE_LOOP ( 'NONE', ( #8067, #11976 ) ) ;
#7559 = FACE_OUTER_BOUND ( 'NONE', #4837, .T. ) ;
#7561 = ADVANCED_FACE ( 'NONE', ( #1251 ), #9668, .F. ) ;
#7562 = ORIENTED_EDGE ( 'NONE', *, *, #14148, .F. ) ;
#7563 = AXIS2_PLACEMENT_3D ( 'NONE', #6595, #7678, #12359 ) ;
#7564 = CARTESIAN_POINT ( 'NONE',  ( -21.49969986081095996, -67.00737899243799234, -5.497689735156006563 ) ) ;
#7565 = CARTESIAN_POINT ( 'NONE',  ( -14.61203582817000068, -107.1622034095870077, -6.087689735155999315 ) ) ;
#7566 = MANIFOLD_SOLID_BREP ( 'Stock-MAS-672-1', #4877 ) ;
#7567 = VECTOR ( 'NONE', #12648, 1000.000000000000000 ) ;
#7568 = DIRECTION ( 'NONE',  ( 0.6061090314441981430, -0.7953815700667045130, 9.612616959383179548E-16 ) ) ;
#7569 = DIRECTION ( 'NONE',  ( 0.000000000000000000, 1.000000000000000000, 1.224646799147350002E-16 ) ) ;
#7570 = EDGE_CURVE ( 'NONE', #11046, #9250, #2696, .T. ) ;
#7571 = CARTESIAN_POINT ( 'NONE',  ( 2.500300139188999182, -46.50737899243799944, 44.50231026484399877 ) ) ;
#7572 = EDGE_CURVE ( 'NONE', #7870, #14077, #5, .T. ) ;
#7573 = DIRECTION ( 'NONE',  ( 1.000000000000000000, 0.000000000000000000, 0.000000000000000000 ) ) ;
#7574 = FACE_OUTER_BOUND ( 'NONE', #14099, .T. ) ;
#7575 = CARTESIAN_POINT ( 'NONE',  ( -7.515340199219564532, -44.00737819808650642, 44.63626335271796819 ) ) ;
#7576 = ORIENTED_EDGE ( 'NONE', *, *, #13065, .T. ) ;
#7577 = CARTESIAN_POINT ( 'NONE',  ( -15.49969986081092088, -13.50737899243822504, 56.85231026484398598 ) ) ;
#7578 = CIRCLE ( 'NONE', #993, 9.974999999999999645 ) ;
#7579 = ORIENTED_EDGE ( 'NONE', *, *, #13545, .F. ) ;
#7580 = DIRECTION ( 'NONE',  ( 0.000000000000000000, -1.000000000000000000, -1.224646799147350002E-16 ) ) ;
#7582 = EDGE_LOOP ( 'NONE', ( #5774, #14518, #11334, #1227 ) ) ;
#7581 = LINE ( 'NONE', #11107, #6176 ) ;
#7583 = ORIENTED_EDGE ( 'NONE', *, *, #5415, .F. ) ;
#7584 = CARTESIAN_POINT ( 'NONE',  ( -15.49969986081092088, -13.50737899243822504, 56.85231026484398598 ) ) ;
#7585 = CARTESIAN_POINT ( 'NONE',  ( -22.13265177292497299, -18.11337496850924822, 56.85231026484398598 ) ) ;
#7587 = ORIENTED_EDGE ( 'NONE', *, *, #7093, .F. ) ;
#7586 = CARTESIAN_POINT ( 'NONE',  ( -15.49969986081099194, -27.00737899243800300, 19.50231026484399877 ) ) ;
#7588 = CARTESIAN_POINT ( 'NONE',  ( -15.49969986081099727, -27.00737899243800300, 2.502310264843997878 ) ) ;
#7589 = DIRECTION ( 'NONE',  ( -1.000000000000000000, -1.201369187114119994E-15, -9.616040805000176517E-16 ) ) ;
#7590 = CARTESIAN_POINT ( 'NONE',  ( -7.711221940648826489, -11.37542292179617753, 56.85231026484400019 ) ) ;
#7591 = EDGE_CURVE ( 'NONE', #13132, #7744, #12894, .T. ) ;
#7592 = EDGE_CURVE ( 'NONE', #2975, #11290, #120, .T. ) ;
#7594 = PLANE ( 'NONE',  #8402 ) ;
#7593 = CARTESIAN_POINT ( 'NONE',  ( -20.59651154950486784, -18.41489981358536809, 57.00231026484397745 ) ) ;
#7595 = ORIENTED_EDGE ( 'NONE', *, *, #12266, .F. ) ;
#7596 = DIRECTION ( 'NONE',  ( 0.000000000000000000, -1.000000000000000000, 0.000000000000000000 ) ) ;
#7597 = DIRECTION ( 'NONE',  ( -0.8772189822852959340, 0.4800904676395371662, -9.902680687415702019E-16 ) ) ;
#7598 = ORIENTED_EDGE ( 'NONE', *, *, #14088, .F. ) ;
#7599 = ORIENTED_EDGE ( 'NONE', *, *, #12253, .T. ) ;
#7600 = FACE_OUTER_BOUND ( 'NONE', #383, .T. ) ;
#7601 = AXIS2_PLACEMENT_3D ( 'NONE', #4745, #11418, #12576 ) ;
#7602 = EDGE_LOOP ( 'NONE', ( #4449, #10116, #13851 ) ) ;
#7604 = ADVANCED_FACE ( 'NONE', ( #5906 ), #6058, .T. ) ;
#7603 = CARTESIAN_POINT ( 'NONE',  ( -7.838474667259318629, -46.81609114312938402, -7.983182814980946063 ) ) ;
#7605 = DIRECTION ( 'NONE',  ( -8.673617379884027583E-16, 1.000000000000000000, 0.000000000000000000 ) ) ;
#7606 = DIRECTION ( 'NONE',  ( 0.000000000000000000, 1.000000000000000000, 1.224646799147350002E-16 ) ) ;
#7607 = VECTOR ( 'NONE', #7718, 1000.000000000000000 ) ;
#7608 = CARTESIAN_POINT ( 'NONE',  ( -34.99969986081099904, -20.37340439622244048, -12.52892449124999885 ) ) ;
#7609 = DIRECTION ( 'NONE',  ( 0.5975035461963189576, 0.8018662683283437342, 0.000000000000000000 ) ) ;
#7610 = CARTESIAN_POINT ( 'NONE',  ( -7.731023390221355207, -11.30308411758414877, 56.85231026484400019 ) ) ;
#7611 = ORIENTED_EDGE ( 'NONE', *, *, #2059, .F. ) ;
#7612 = DIRECTION ( 'NONE',  ( 8.018662683283438208E-16, -5.975035461963189015E-16, -1.000000000000000000 ) ) ;
#7613 = DIRECTION ( 'NONE',  ( 1.000000000000000000, 1.201369187114119994E-15, 9.616040805000176517E-16 ) ) ;
#7614 = ORIENTED_EDGE ( 'NONE', *, *, #11117, .T. ) ;
#7615 = VECTOR ( 'NONE', #2421, 1000.000000000000114 ) ;
#7616 = CARTESIAN_POINT ( 'NONE',  ( -15.49969986081091378, -13.50737899243822859, 51.00231026484399166 ) ) ;
#7617 = EDGE_LOOP ( 'NONE', ( #4540, #518 ) ) ;
#7618 = CARTESIAN_POINT ( 'NONE',  ( -2.716578225681299141, -32.00737899243799944, -15.75165123257469801 ) ) ;
#7619 = AXIS2_PLACEMENT_3D ( 'NONE', #11921, #1517, #4968 ) ;
#7620 = ADVANCED_FACE ( 'NONE', ( #8440 ), #1966, .T. ) ;
#7621 = PLANE ( 'NONE',  #9269 ) ;
#7622 = CARTESIAN_POINT ( 'NONE',  ( -7.662963790453772184, -48.42200951437349943, 17.89473638362698082 ) ) ;
#7623 = AXIS2_PLACEMENT_3D ( 'NONE', #3538, #7195, #1240 ) ;
#7624 = CARTESIAN_POINT ( 'NONE',  ( -8.992083836519068285, -50.38952316532491693, -11.37983390804291517 ) ) ;
#7625 = DIRECTION ( 'NONE',  ( -0.3633925226508256667, 0.9316361277244830097, -8.480480961564259036E-16 ) ) ;
#7626 = ORIENTED_EDGE ( 'NONE', *, *, #6588, .F. ) ;
#7627 = DIRECTION ( 'NONE',  ( -1.000000000000000000, 0.000000000000000000, 0.000000000000000000 ) ) ;
#7628 = CARTESIAN_POINT ( 'NONE',  ( -7.694370900912546496, -46.24434200338747303, -3.010997809292743632 ) ) ;
#7629 = ORIENTED_EDGE ( 'NONE', *, *, #3003, .F. ) ;
#7631 = ORIENTED_EDGE ( 'NONE', *, *, #14302, .T. ) ;
#7630 = CARTESIAN_POINT ( 'NONE',  ( -15.49969986081099904, -32.00737899243799944, 24.21206422150100224 ) ) ;
#7632 = ORIENTED_EDGE ( 'NONE', *, *, #1787, .F. ) ;
#7633 = ADVANCED_FACE ( 'NONE', ( #191 ), #2631, .F. ) ;
#7634 = DIRECTION ( 'NONE',  ( 0.000000000000000000, 0.000000000000000000, 1.000000000000000000 ) ) ;
#7635 = ORIENTED_EDGE ( 'NONE', *, *, #14783, .T. ) ;
#7636 = VECTOR ( 'NONE', #14682, 1000.000000000000000 ) ;
#7637 = EDGE_CURVE ( 'NONE', #964, #12427, #2460, .T. ) ;
#7638 = CARTESIAN_POINT ( 'NONE',  ( -15.49969986081091200, -13.50737899243823037, 48.00231026484398456 ) ) ;
#7639 = CARTESIAN_POINT ( 'NONE',  ( -23.49969986081099904, -44.50737899243799944, -109.5506571639849938 ) ) ;
#7640 = DIRECTION ( 'NONE',  ( -0.1960948578651675878, 0.9805849309054466278, -7.431448254773955467E-16 ) ) ;
#7641 = DIRECTION ( 'NONE',  ( 0.000000000000000000, 0.000000000000000000, -1.000000000000000000 ) ) ;
#7642 = LINE ( 'NONE', #3138, #13142 ) ;
#7643 = AXIS2_PLACEMENT_3D ( 'NONE', #5257, #3887, #10851 ) ;
#7644 = DIRECTION ( 'NONE',  ( -8.018662683283438208E-16, 5.975035461963189015E-16, 1.000000000000000000 ) ) ;
#7645 = VERTEX_POINT ( 'NONE', #6290 ) ;
#7646 = LINE ( 'NONE', #338, #2480 ) ;
#7647 = AXIS2_PLACEMENT_3D ( 'NONE', #9980, #3178, #4176 ) ;
#7648 = EDGE_LOOP ( 'NONE', ( #8511, #9990 ) ) ;
#7649 = CARTESIAN_POINT ( 'NONE',  ( -6.368730986314236731, -9.491655842995191605, 54.00231026484399166 ) ) ;
#7651 = VERTEX_POINT ( 'NONE', #13345 ) ;
#7650 = DIRECTION ( 'NONE',  ( 0.5975035461963189576, 0.8018662683283437342, 0.000000000000000000 ) ) ;
#7652 = ORIENTED_EDGE ( 'NONE', *, *, #13272, .F. ) ;
#7653 = EDGE_CURVE ( 'NONE', #2329, #1607, #13218, .T. ) ;
#7654 = DIRECTION ( 'NONE',  ( -1.000000000000000000, -3.700743415417188632E-16, 0.000000000000000000 ) ) ;
#7655 = EDGE_CURVE ( 'NONE', #6300, #2715, #11034, .T. ) ;
#7657 = VERTEX_POINT ( 'NONE', #13420 ) ;
#7656 = LINE ( 'NONE', #10832, #362 ) ;
#7658 = CARTESIAN_POINT ( 'NONE',  ( -11.23011178639221086, -12.05596824276080348, -13.04425562498458291 ) ) ;
#7659 = ADVANCED_FACE ( 'NONE', ( #3005 ), #563, .T. ) ;
#7660 = DIRECTION ( 'NONE',  ( 1.982541115402064518E-15, -0.1872998510044552312, -0.9823027872370662106 ) ) ;
#7661 = LINE ( 'NONE', #8664, #14138 ) ;
#7662 = EDGE_CURVE ( 'NONE', #1400, #9211, #14664, .T. ) ;
#7663 = VECTOR ( 'NONE', #7930, 1000.000000000000000 ) ;
#7664 = DIRECTION ( 'NONE',  ( 0.1855175943453168941, 0.9826409426582662920, -4.383711467890769768E-16 ) ) ;
#7665 = ORIENTED_EDGE ( 'NONE', *, *, #6524, .F. ) ;
#7666 = DIRECTION ( 'NONE',  ( 8.018662683283438208E-16, -5.975035461963189015E-16, -1.000000000000000000 ) ) ;
#7667 = ORIENTED_EDGE ( 'NONE', *, *, #14899, .T. ) ;
#7668 = CARTESIAN_POINT ( 'NONE',  ( -25.49893968439952729, -13.50738396921345519, 60.35575980305132049 ) ) ;
#7669 = ORIENTED_EDGE ( 'NONE', *, *, #515, .T. ) ;
#7670 = ORIENTED_EDGE ( 'NONE', *, *, #5334, .F. ) ;
#7671 = VECTOR ( 'NONE', #14902, 1000.000000000000227 ) ;
#7672 = CARTESIAN_POINT ( 'NONE',  ( -7.707227416580196611, -8.855645637450560770, 56.85231026484400019 ) ) ;
#7673 = EDGE_CURVE ( 'NONE', #4906, #4831, #636, .T. ) ;
#7674 = VERTEX_POINT ( 'NONE', #9890 ) ;
#7675 = CARTESIAN_POINT ( 'NONE',  ( -25.44713467170207366, -12.76632185356751847, 54.00231026484397745 ) ) ;
#7676 = EDGE_CURVE ( 'NONE', #3314, #10056, #3918, .T. ) ;
#7677 = B_SPLINE_CURVE_WITH_KNOTS ( 'NONE', 3,
 ( #9167, #13696, #3211, #920, #12627, #7858, #12554, #1838, #5648, #6563, #5571, #14915, #9092, #14688, #13772, #3292, #7940, #10320, #4516, #11170, #4209, #3055, #7709, #1918, #11248, #5425, #9319, #5867, #11765, #1137, #10396, #229 ),
 .UNSPECIFIED., .F., .F.,
 ( 4, 2, 2, 2, 2, 2, 2, 2, 2, 2, 2, 2, 2, 2, 2, 4 ),
 ( 0.007859347252422295774, 0.008369889772020241286, 0.008880432291618185064, 0.009390974811216130577, 0.009901517330814076090, 0.01041205985041202160, 0.01092260237000996538, 0.01143314488960791089, 0.01194368740920585641, 0.01296477244840174570, 0.01347531496799970509, 0.01398585748759766448, 0.01449640000719562213, 0.01500694252679357979, 0.01551748504639154091, 0.01602802756598949857 ),
 .UNSPECIFIED. ) ;
#7678 = DIRECTION ( 'NONE',  ( 0.8660254037844387076, -0.4999999999999998890, 0.000000000000000000 ) ) ;
#7679 = VECTOR ( 'NONE', #11849, 999.9999999999998863 ) ;
#7680 = FACE_OUTER_BOUND ( 'NONE', #13501, .T. ) ;
#7681 = EDGE_CURVE ( 'NONE', #5664, #2729, #1705, .T. ) ;
#7682 = DIRECTION ( 'NONE',  ( 0.000000000000000000, 1.131341397376178572E-16, -1.000000000000000000 ) ) ;
#7683 = DIRECTION ( 'NONE',  ( -7.070501591499349439E-17, 0.000000000000000000, 1.000000000000000000 ) ) ;
#7684 = VERTEX_POINT ( 'NONE', #2933 ) ;
#7685 = DIRECTION ( 'NONE',  ( 0.5975035461963187355, 0.8018662683283439563, 0.000000000000000000 ) ) ;
#7686 = ORIENTED_EDGE ( 'NONE', *, *, #2556, .F. ) ;
#7687 = DIRECTION ( 'NONE',  ( -0.9755678736739583634, 0.2196982563774038943, -9.135454576426008610E-16 ) ) ;
#7688 = CARTESIAN_POINT ( 'NONE',  ( -23.14528701667493849, -16.10665716956490812, 56.85231026484398598 ) ) ;
#7689 = CARTESIAN_POINT ( 'NONE',  ( -15.49969986081100082, -19.50737899243800300, 19.50231026484399877 ) ) ;
#7690 = ORIENTED_EDGE ( 'NONE', *, *, #3781, .T. ) ;
#7691 = DIRECTION ( 'NONE',  ( -8.018662683283439195E-16, 5.975035461963190001E-16, 1.000000000000000000 ) ) ;
#7692 = LINE ( 'NONE', #6467, #727 ) ;
#7693 = PRODUCT_CONTEXT ( 'NONE', #13111, 'mechanical' ) ;
#7694 = LINE ( 'NONE', #11153, #421 ) ;
#7695 = ADVANCED_FACE ( 'NONE', ( #9744 ), #6436, .F. ) ;
#7696 = CARTESIAN_POINT ( 'NONE',  ( -15.49969986081091022, -13.50737899243823215, 45.50231026484398456 ) ) ;
#7697 = DIRECTION ( 'NONE',  ( -8.018662683283438208E-16, 5.975035461963189015E-16, 1.000000000000000000 ) ) ;
#7698 = ORIENTED_EDGE ( 'NONE', *, *, #2120, .T. ) ;
#7699 = PLANE ( 'NONE',  #7006 ) ;
#7700 = CIRCLE ( 'NONE', #1119, 1.600959456836780204 ) ;
#7701 = PLANE ( 'NONE',  #10953 ) ;
#7702 = ORIENTED_EDGE ( 'NONE', *, *, #2573, .T. ) ;
#7704 = ORIENTED_EDGE ( 'NONE', *, *, #10855, .T. ) ;
#7703 = CARTESIAN_POINT ( 'NONE',  ( -34.68185672695825872, -38.77348753601568632, -12.72054782938013062 ) ) ;
#7705 = ORIENTED_EDGE ( 'NONE', *, *, #12807, .T. ) ;
#7706 = CARTESIAN_POINT ( 'NONE',  ( -15.61203582816999891, -108.2036686363109084, -6.241690937583108223 ) ) ;
#7707 = CARTESIAN_POINT ( 'NONE',  ( -7.704840168542555823, -46.32660887508429681, 56.18327162512064632 ) ) ;
#7708 = DIRECTION ( 'NONE',  ( -0.1960948578651647567, 0.9805849309054472940, -7.431448254773936732E-16 ) ) ;
#7709 = CARTESIAN_POINT ( 'NONE',  ( -8.493401964816579053, -48.37115091595966732, 46.17630167696805898 ) ) ;
#7710 = VECTOR ( 'NONE', #5576, 1000.000000000000000 ) ;
#7711 = FACE_BOUND ( 'NONE', #6685, .T. ) ;
#7712 = ADVANCED_FACE ( 'NONE', ( #12114 ), #8663, .T. ) ;
#7713 = CARTESIAN_POINT ( 'NONE',  ( -23.40321606353253614, -15.16438883951732741, 57.00231026484397745 ) ) ;
#7714 = LINE ( 'NONE', #696, #6926 ) ;
#7715 = DIRECTION ( 'NONE',  ( 0.000000000000000000, -2.220446049250312588E-16, 1.000000000000000000 ) ) ;
#7716 = ADVANCED_FACE ( 'NONE', ( #5373 ), #8890, .T. ) ;
#7717 = ORIENTED_EDGE ( 'NONE', *, *, #7113, .F. ) ;
#7718 = DIRECTION ( 'NONE',  ( -1.000000000000000078E-15, 1.000000000000000000, 0.000000000000000000 ) ) ;
#7719 = VECTOR ( 'NONE', #11767, 1000.000000000000000 ) ;
#7720 = ORIENTED_EDGE ( 'NONE', *, *, #2990, .F. ) ;
#7721 = LINE ( 'NONE', #8078, #14398 ) ;
#7723 = VERTEX_POINT ( 'NONE', #9958 ) ;
#7722 = CARTESIAN_POINT ( 'NONE',  ( -16.39856880423293006, -20.52544743201270450, 57.00231026484399166 ) ) ;
#7724 = ORIENTED_EDGE ( 'NONE', *, *, #2453, .T. ) ;
#7725 = CARTESIAN_POINT ( 'NONE',  ( -28.28282149594069850, -32.00737899243799944, 54.75627176226269199 ) ) ;
#7727 = ORIENTED_EDGE ( 'NONE', *, *, #5788, .F. ) ;
#7726 = DIRECTION ( 'NONE',  ( -0.1855175943453168941, -0.9826409426582662920, 4.383711467890769768E-16 ) ) ;
#7728 = LINE ( 'NONE', #12571, #240 ) ;
#7729 = CARTESIAN_POINT ( 'NONE',  ( -15.49969986081092088, -13.50737899243822504, 56.85231026484398598 ) ) ;
#7730 = CIRCLE ( 'NONE', #12399, 2.500000000000002220 ) ;
#7731 = ADVANCED_FACE ( 'NONE', ( #7512 ), #4155, .T. ) ;
#7732 = EDGE_CURVE ( 'NONE', #6817, #5856, #13569, .T. ) ;
#7733 = PLANE ( 'NONE',  #7601 ) ;
#7734 = COLOUR_RGB ( '', 0.40784314, 0.44705882, 0.49803922) ;
#7735 = DIRECTION ( 'NONE',  ( -0.5975035461963189576, -0.8018662683283438453, 9.860761315262649757E-32 ) ) ;
#7736 = EDGE_CURVE ( 'NONE', #1870, #3162, #1231, .T. ) ;
#7737 = VERTEX_POINT ( 'NONE', #1629 ) ;
#7738 = DIRECTION ( 'NONE',  ( -0.3956847857120157075, 0.9183863840214729901, -8.660254037844388394E-16 ) ) ;
#7739 = VERTEX_POINT ( 'NONE', #6505 ) ;
#7740 = CARTESIAN_POINT ( 'NONE',  ( -15.49969986081099904, 22.99262100756199700, 40.08706422150100224 ) ) ;
#7741 = ORIENTED_EDGE ( 'NONE', *, *, #5599, .T. ) ;
#7742 = ORIENTED_EDGE ( 'NONE', *, *, #7456, .F. ) ;
#7743 = FACE_BOUND ( 'NONE', #1902, .T. ) ;
#7744 = VERTEX_POINT ( 'NONE', #12267 ) ;
#7745 = CIRCLE ( 'NONE', #12149, 9.974999999999999645 ) ;
#7746 = ADVANCED_FACE ( 'NONE', ( #13273 ), #2782, .T. ) ;
#7747 = CARTESIAN_POINT ( 'NONE',  ( -12.91865582312666838, -36.91712645767735523, 56.91652338071235562 ) ) ;
#7748 = CIRCLE ( 'NONE', #441, 4.999999999999997335 ) ;
#7749 = FACE_BOUND ( 'NONE', #381, .T. ) ;
#7750 = CARTESIAN_POINT ( 'NONE',  ( -15.09158957740191553, -107.4899781488447843, -7.806719612820868903 ) ) ;
#7751 = EDGE_CURVE ( 'NONE', #9903, #14455, #941, .T. ) ;
#7752 = DIRECTION ( 'NONE',  ( 0.5975035461963188466, 0.8018662683283437342, 0.000000000000000000 ) ) ;
#7753 = EDGE_CURVE ( 'NONE', #12040, #2877, #7879, .T. ) ;
#7754 = AXIS2_PLACEMENT_3D ( 'NONE', #4198, #12310, #4355 ) ;
#7755 = VECTOR ( 'NONE', #11199, 1000.000000000000000 ) ;
#7756 = DIRECTION ( 'NONE',  ( -8.018662683283438208E-16, 5.975035461963189015E-16, 1.000000000000000000 ) ) ;
#7758 = CARTESIAN_POINT ( 'NONE',  ( 5.018124931134533284, 5.923502402102436726, 29.47442983242405745 ) ) ;
#7757 = CARTESIAN_POINT ( 'NONE',  ( 4.000300139189000959, -19.50737899243798879, -12.52892449124999885 ) ) ;
#7759 = VECTOR ( 'NONE', #4511, 1000.000000000000227 ) ;
#7760 = EDGE_LOOP ( 'NONE', ( #10598, #2790, #12292, #6758, #14349, #9931 ) ) ;
#7761 = DIRECTION ( 'NONE',  ( 0.000000000000000000, -1.334178587669858246E-16, 1.000000000000000000 ) ) ;
#7762 = CYLINDRICAL_SURFACE ( 'NONE', #2172, 0.4500000000000011768 ) ;
#7763 = EDGE_LOOP ( 'NONE', ( #12886, #9759, #8504, #6409 ) ) ;
#7764 = CARTESIAN_POINT ( 'NONE',  ( -15.11203582817000068, -107.1622034095870077, -6.087689735156000204 ) ) ;
#7765 = CARTESIAN_POINT ( 'NONE',  ( 21.89425379661516047, -25.37906976104908452, 27.03274040250693488 ) ) ;
#7766 = DIRECTION ( 'NONE',  ( 1.000000000000000000, -3.922012711866029438E-32, 3.202566417187950042E-16 ) ) ;
#7767 = ORIENTED_EDGE ( 'NONE', *, *, #15036, .T. ) ;
#7768 = LINE ( 'NONE', #14967, #7132 ) ;
#7769 = LINE ( 'NONE', #827, #4383 ) ;
#7770 = PRODUCT_CONTEXT ( 'NONE', #10759, 'mechanical' ) ;
#7771 = CARTESIAN_POINT ( 'NONE',  ( -23.59767874945767119, -17.60420555931063902, 56.85231026484398598 ) ) ;
#7772 = VECTOR ( 'NONE', #5988, 1000.000000000000114 ) ;
#7773 = DIRECTION ( 'NONE',  ( -8.018662683283438208E-16, 5.975035461963189015E-16, 1.000000000000000000 ) ) ;
#7774 = CARTESIAN_POINT ( 'NONE',  ( -22.56290636796585503, -13.91571566392944526, 56.85231026484398598 ) ) ;
#7775 = ADVANCED_FACE ( 'NONE', ( #13713 ), #3233, .T. ) ;
#7776 = ORIENTED_EDGE ( 'NONE', *, *, #11151, .T. ) ;
#7777 = CARTESIAN_POINT ( 'NONE',  ( -33.23380676216500973, 7.699995122771584377, 31.04377206689012425 ) ) ;
#7778 = CARTESIAN_POINT ( 'NONE',  ( -23.49969986081099904, -44.50737899243799944, -5.497689735156002122 ) ) ;
#7779 = ORIENTED_EDGE ( 'NONE', *, *, #12567, .F. ) ;
#7781 = ORIENTED_EDGE ( 'NONE', *, *, #117, .T. ) ;
#7780 = CARTESIAN_POINT ( 'NONE',  ( -20.54757852167729837, -19.81012014412530320, 56.85231026484398598 ) ) ;
#7782 = VERTEX_POINT ( 'NONE', #13639 ) ;
#7783 = CARTESIAN_POINT ( 'NONE',  ( -24.28571865450477318, -8.784403367172064492, 54.00231026484397745 ) ) ;
#7784 = CARTESIAN_POINT ( 'NONE',  ( -12.92191964973194906, -52.08526088413143640, 56.91445648935585666 ) ) ;
#7785 = EDGE_CURVE ( 'NONE', #13801, #2422, #786, .T. ) ;
#7786 = ADVANCED_FACE ( 'NONE', ( #8958 ), #15082, .F. ) ;
#7787 = CARTESIAN_POINT ( 'NONE',  ( 7.000300139189000070, -32.00737899243799944, 24.21206422150099868 ) ) ;
#7788 = DIRECTION ( 'NONE',  ( -8.018662683283438208E-16, 5.975035461963189015E-16, 1.000000000000000000 ) ) ;
#7789 = LINE ( 'NONE', #11395, #2851 ) ;
#7790 = CARTESIAN_POINT ( 'NONE',  ( -15.80242800153736837, -16.08775797096295435, 51.00231026484399166 ) ) ;
#7791 = CARTESIAN_POINT ( 'NONE',  ( -38.29214122569165824, 4.584400081984788322, 21.07650941979234815 ) ) ;
#7792 = CIRCLE ( 'NONE', #8282, 1.769239858347549932 ) ;
#7793 = LINE ( 'NONE', #1142, #1292 ) ;
#7794 = ORIENTED_EDGE ( 'NONE', *, *, #5649, .T. ) ;
#7795 = CARTESIAN_POINT ( 'NONE',  ( 17.66550352352905406, -29.89979048896684688, 41.71521872389765662 ) ) ;
#7796 = EDGE_LOOP ( 'NONE', ( #3825, #1398, #9696, #1189 ) ) ;
#7797 = EDGE_LOOP ( 'NONE', ( #11241, #170, #10789, #2815 ) ) ;
#7798 = EDGE_LOOP ( 'NONE', ( #10023, #8279, #13417, #8818 ) ) ;
#7799 = CARTESIAN_POINT ( 'NONE',  ( -15.49969986081091733, -13.50737899243822682, 54.00231026484399166 ) ) ;
#7800 = ORIENTED_EDGE ( 'NONE', *, *, #7230, .F. ) ;
#7801 = DIRECTION ( 'NONE',  ( 0.000000000000000000, 0.000000000000000000, -1.000000000000000000 ) ) ;
#7802 = EDGE_CURVE ( 'NONE', #13942, #3312, #4380, .T. ) ;
#7803 = DIRECTION ( 'NONE',  ( 8.018662683283438208E-16, -5.975035461963189015E-16, -1.000000000000000000 ) ) ;
#7804 = AXIS2_PLACEMENT_3D ( 'NONE', #2849, #7589, #7660 ) ;
#7805 = CYLINDRICAL_SURFACE ( 'NONE', #13477, 2.499999999999998668 ) ;
#7806 = CARTESIAN_POINT ( 'NONE',  ( -28.28282149594069850, -32.00737899243799944, -15.75165123257469801 ) ) ;
#7807 = ORIENTED_EDGE ( 'NONE', *, *, #1803, .F. ) ;
#7808 = CARTESIAN_POINT ( 'NONE',  ( 17.94020077395062174, -24.45836243756893325, 41.18425341717939148 ) ) ;
#7809 = VERTEX_POINT ( 'NONE', #10105 ) ;
#7810 = DIRECTION ( 'NONE',  ( 0.5975035461963189576, 0.8018662683283437342, 0.000000000000000000 ) ) ;
#7811 = VERTEX_POINT ( 'NONE', #6657 ) ;
#7812 = VERTEX_POINT ( 'NONE', #11342 ) ;
#7813 = CARTESIAN_POINT ( 'NONE',  ( -15.49969986081099016, -27.00737899243800300, 27.50231026484399877 ) ) ;
#7814 = ORIENTED_EDGE ( 'NONE', *, *, #13728, .T. ) ;
#7815 = CARTESIAN_POINT ( 'NONE',  ( -7.552314780320042331, -43.45227698143176553, 56.15064027656714529 ) ) ;
#7816 = EDGE_CURVE ( 'NONE', #8987, #6022, #864, .T. ) ;
#7817 = ADVANCED_FACE ( 'NONE', ( #4610 ), #12573, .F. ) ;
#7818 = CARTESIAN_POINT ( 'NONE',  ( -10.19146053163822963, -90.54589302285323527, -6.344455741628062029 ) ) ;
#7819 = CARTESIAN_POINT ( 'NONE',  ( -23.08034316846174150, -10.72437754756471762, 56.85231026484398598 ) ) ;
#7820 = VECTOR ( 'NONE', #14000, 1000.000000000000114 ) ;
#7821 = CARTESIAN_POINT ( 'NONE',  ( -15.49969986081099904, 20.99262100756200411, 8.587064221501000461 ) ) ;
#7823 = CYLINDRICAL_SURFACE ( 'NONE', #13161, 0.4500000000000011768 ) ;
#7822 = CARTESIAN_POINT ( 'NONE',  ( -12.73873237239188683, -12.31782212615591021, 57.00231026484397745 ) ) ;
#7824 = ORIENTED_EDGE ( 'NONE', *, *, #1317, .F. ) ;
#7825 = CARTESIAN_POINT ( 'NONE',  ( -12.37415300023346454, -4.034703455804748984, 54.00231026484399166 ) ) ;
#7826 = CYLINDRICAL_SURFACE ( 'NONE', #8265, 5.000000000000000000 ) ;
#7827 = EDGE_CURVE ( 'NONE', #3090, #2942, #752, .T. ) ;
#7828 = ORIENTED_EDGE ( 'NONE', *, *, #10567, .F. ) ;
#7829 = VERTEX_POINT ( 'NONE', #8036 ) ;
#7830 = DIRECTION ( 'NONE',  ( 1.011922027653136551E-15, -1.000000000000000000, 0.000000000000000000 ) ) ;
#7831 = CARTESIAN_POINT ( 'NONE',  ( -15.49969986081092088, -13.50737899243822504, 56.85231026484398598 ) ) ;
#7832 = ORIENTED_EDGE ( 'NONE', *, *, #4982, .T. ) ;
#7833 = DIRECTION ( 'NONE',  ( -0.4224988092984270360, -0.5670050759397227136, 0.7071067811865480168 ) ) ;
#7834 = EDGE_CURVE ( 'NONE', #505, #7429, #10338, .T. ) ;
#7835 = EDGE_CURVE ( 'NONE', #11757, #6457, #11489, .T. ) ;
#7836 = CIRCLE ( 'NONE', #2740, 28.00000000000000000 ) ;
#7837 = DIRECTION ( 'NONE',  ( -1.000000000000000000, -1.000000000000000078E-15, -1.000000000000000078E-15 ) ) ;
#7838 = APPLICATION_PROTOCOL_DEFINITION ( 'draft international standard', 'automotive_design', 1998, #8688 ) ;
#7839 = CARTESIAN_POINT ( 'NONE',  ( -7.869402401355066523, -47.25089185752115384, 21.90682449334191162 ) ) ;
#7840 = LINE ( 'NONE', #2965, #14561 ) ;
#7841 = CARTESIAN_POINT ( 'NONE',  ( -18.93133274217424855, -21.90887563098697655, 56.85231026484400019 ) ) ;
#7842 = CIRCLE ( 'NONE', #3955, 37.50000000000000000 ) ;
#7843 = VERTEX_POINT ( 'NONE', #4456 ) ;
#7844 = DIRECTION ( 'NONE',  ( -0.9918751611018171710, -0.1272150336605075427, -7.193398003386516820E-16 ) ) ;
#7845 = CARTESIAN_POINT ( 'NONE',  ( -7.506834498223213359, -44.86600688595157749, -3.611780095971914850 ) ) ;
#7846 = CARTESIAN_POINT ( 'NONE',  ( -22.33089034576175180, -8.323646113680169378, 56.85231026484398598 ) ) ;
#7847 = AXIS2_PLACEMENT_3D ( 'NONE', #255, #3616, #8350 ) ;
#7848 = ORIENTED_EDGE ( 'NONE', *, *, #9495, .T. ) ;
#7850 = ORIENTED_EDGE ( 'NONE', *, *, #248, .T. ) ;
#7849 = CARTESIAN_POINT ( 'NONE',  ( 7.500245791298697284, 3.992621007561997892, 24.26206422150100295 ) ) ;
#7851 = ORIENTED_EDGE ( 'NONE', *, *, #7835, .T. ) ;
#7852 = CARTESIAN_POINT ( 'NONE',  ( 4.000300139189000959, -20.37340439622241917, -12.52892449124999885 ) ) ;
#7853 = CARTESIAN_POINT ( 'NONE',  ( -14.96933016362806690, -52.50737899243799234, 57.00231026484399166 ) ) ;
#7854 = ADVANCED_FACE ( 'NONE', ( #13792 ), #2166, .T. ) ;
#7855 = EDGE_CURVE ( 'NONE', #8000, #4906, #4534, .T. ) ;
#7856 = VECTOR ( 'NONE', #13966, 1000.000000000000114 ) ;
#7857 = DIRECTION ( 'NONE',  ( 3.202566417187950042E-16, 1.224646799147350002E-16, -1.000000000000000000 ) ) ;
#7858 = CARTESIAN_POINT ( 'NONE',  ( -8.123284869591744339, -47.60801320870127995, 42.25191011081004433 ) ) ;
#7859 = VECTOR ( 'NONE', #12698, 1000.000000000000000 ) ;
#7860 = AXIS2_PLACEMENT_3D ( 'NONE', #4640, #11596, #1112 ) ;
#7861 = VECTOR ( 'NONE', #5115, 1000.000000000000000 ) ;
#7862 = CARTESIAN_POINT ( 'NONE',  ( -24.80452494096261873, -9.912819877918101596, 56.85231026484398598 ) ) ;
#7863 = CARTESIAN_POINT ( 'NONE',  ( -9.376966593418606166, -18.77214511605354019, 57.00231026484399166 ) ) ;
#7864 = DIRECTION ( 'NONE',  ( -0.3306575217771128283, 0.9437508163134049610, -8.290375725550417844E-16 ) ) ;
#7865 = EDGE_CURVE ( 'NONE', #11873, #12154, #5747, .T. ) ;
#7866 = CARTESIAN_POINT ( 'NONE',  ( -16.48891182509095543, -11.21141303238454334, 51.25231026484399166 ) ) ;
#7867 = VERTEX_POINT ( 'NONE', #5819 ) ;
#7868 = CARTESIAN_POINT ( 'NONE',  ( -12.84086554789186607, -5.882298658668338120, 56.85231026484398598 ) ) ;
#7869 = AXIS2_PLACEMENT_3D ( 'NONE', #7969, #12503, #3252 ) ;
#7870 = VERTEX_POINT ( 'NONE', #1156 ) ;
#7871 = LINE ( 'NONE', #12563, #9698 ) ;
#7873 = EDGE_LOOP ( 'NONE', ( #11980, #3523, #13488, #6406 ) ) ;
#7872 = DIRECTION ( 'NONE',  ( 0.000000000000000000, -9.251858538542971581E-17, 1.000000000000000000 ) ) ;
#7874 = EDGE_LOOP ( 'NONE', ( #87, #1110, #1331, #9796 ) ) ;
#7875 = AXIS2_PLACEMENT_3D ( 'NONE', #3241, #869, #9350 ) ;
#7876 = CARTESIAN_POINT ( 'NONE',  ( -17.87376992080280758, -22.26666214519964271, 57.00231026484399166 ) ) ;
#7877 = ORIENTED_EDGE ( 'NONE', *, *, #4982, .F. ) ;
#7878 = CARTESIAN_POINT ( 'NONE',  ( -20.87112600995945400, -109.8308986703933812, -7.501670736676251394 ) ) ;
#7879 = LINE ( 'NONE', #4305, #7071 ) ;
#7880 = AXIS2_PLACEMENT_3D ( 'NONE', #9676, #14116, #2642 ) ;
#7881 = AXIS2_PLACEMENT_3D ( 'NONE', #6872, #5584, #4676 ) ;
#7882 = AXIS2_PLACEMENT_3D ( 'NONE', #12993, #14285, #9911 ) ;
#7883 = VECTOR ( 'NONE', #14888, 1000.000000000000114 ) ;
#7884 = EDGE_LOOP ( 'NONE', ( #7368, #8784, #1639, #8333 ) ) ;
#7885 = FACE_OUTER_BOUND ( 'NONE', #4680, .T. ) ;
#7886 = ADVANCED_FACE ( 'NONE', ( #5889 ), #11637, .F. ) ;
#7887 = CARTESIAN_POINT ( 'NONE',  ( -20.97295351809511388, -50.34796644937742371, -17.59659479099292412 ) ) ;
#7888 = ORIENTED_EDGE ( 'NONE', *, *, #3707, .F. ) ;
#7889 = CARTESIAN_POINT ( 'NONE',  ( 18.53245405280427960, -27.00737899243800300, 39.96206422150099513 ) ) ;
#7890 = ORIENTED_EDGE ( 'NONE', *, *, #5408, .T. ) ;
#7891 = DIRECTION ( 'NONE',  ( 1.000000000000000000, -1.291538348938060198E-32, 1.054621095516909827E-16 ) ) ;
#7892 = VERTEX_POINT ( 'NONE', #8344 ) ;
#7893 = ORIENTED_EDGE ( 'NONE', *, *, #669, .F. ) ;
#7894 = CARTESIAN_POINT ( 'NONE',  ( -15.49969986081099904, 0.9926210075619987805, 24.21206422150099868 ) ) ;
#7895 = ORIENTED_EDGE ( 'NONE', *, *, #9933, .T. ) ;
#7896 = CARTESIAN_POINT ( 'NONE',  ( -11.26730675207693899, -37.71366398918802787, 56.76333939437698461 ) ) ;
#7897 = VECTOR ( 'NONE', #10137, 1000.000000000000000 ) ;
#7898 = EDGE_CURVE ( 'NONE', #8100, #13349, #13034, .T. ) ;
#7899 = CARTESIAN_POINT ( 'NONE',  ( -24.38380099443793725, -15.36048369738253427, 56.85231026484398598 ) ) ;
#7900 = LINE ( 'NONE', #4628, #977 ) ;
#7901 = VECTOR ( 'NONE', #5468, 1000.000000000000000 ) ;
#7902 = FACE_OUTER_BOUND ( 'NONE', #14743, .T. ) ;
#7903 = VECTOR ( 'NONE', #9348, 1000.000000000000227 ) ;
#7904 = CYLINDRICAL_SURFACE ( 'NONE', #13315, 0.2000000000000012046 ) ;
#7905 = EDGE_CURVE ( 'NONE', #612, #5816, #100, .T. ) ;
#7907 = FACE_OUTER_BOUND ( 'NONE', #6554, .T. ) ;
#7906 = DIRECTION ( 'NONE',  ( -8.018662683283438208E-16, 5.975035461963189015E-16, 1.000000000000000000 ) ) ;
#7908 = VERTEX_POINT ( 'NONE', #1318 ) ;
#7909 = DIRECTION ( 'NONE',  ( -8.018662683283438208E-16, 5.975035461963189015E-16, 1.000000000000000000 ) ) ;
#7910 = CARTESIAN_POINT ( 'NONE',  ( -18.88797976027533920, -16.48321755670100330, -13.13513021181339013 ) ) ;
#7911 = VERTEX_POINT ( 'NONE', #8422 ) ;
#7912 = ORIENTED_EDGE ( 'NONE', *, *, #7751, .F. ) ;
#7913 = CARTESIAN_POINT ( 'NONE',  ( -13.95777467540137806, -22.45074059323463089, 56.85231026484400019 ) ) ;
#7914 = EDGE_CURVE ( 'NONE', #8039, #8731, #270, .T. ) ;
#7915 = CARTESIAN_POINT ( 'NONE',  ( -15.76376720799379427, -36.50737899243800655, -17.99768973515599768 ) ) ;
#7916 = LINE ( 'NONE', #13599, #9869 ) ;
#7917 = VECTOR ( 'NONE', #14919, 1000.000000000000000 ) ;
#7918 = ORIENTED_EDGE ( 'NONE', *, *, #3271, .F. ) ;
#7919 = CARTESIAN_POINT ( 'NONE',  ( -18.18846581869429713, -17.11577719991581148, -13.99768973515600301 ) ) ;
#7920 = PRESENTATION_LAYER_ASSIGNMENT (  '', '', ( #15019 ) ) ;
#7921 = LINE ( 'NONE', #3419, #6323 ) ;
#7922 = DIRECTION ( 'NONE',  ( 0.000000000000000000, 0.1872998510044689147, 0.9823027872370635460 ) ) ;
#7923 = DIRECTION ( 'NONE',  ( 0.5975035461963189576, 0.8018662683283437342, 0.000000000000000000 ) ) ;
#7924 = EDGE_CURVE ( 'NONE', #4803, #2152, #5386, .T. ) ;
#7925 = CARTESIAN_POINT ( 'NONE',  ( -6.426265323245524463, -13.69186664111786200, 56.85231026484400019 ) ) ;
#7926 = ORIENTED_EDGE ( 'NONE', *, *, #9404, .T. ) ;
#7927 = CARTESIAN_POINT ( 'NONE',  ( -10.30965874483576883, -90.56230343551661122, -4.113522448036712298 ) ) ;
#7928 = EDGE_CURVE ( 'NONE', #3880, #1356, #12837, .T. ) ;
#7929 = DIRECTION ( 'NONE',  ( 0.1908089953765451374, -0.5346324819374546067, -0.8232618274527192526 ) ) ;
#7930 = DIRECTION ( 'NONE',  ( -8.018662683283438208E-16, 5.975035461963189015E-16, 1.000000000000000000 ) ) ;
#7931 = VECTOR ( 'NONE', #8110, 1000.000000000000114 ) ;
#7932 = EDGE_CURVE ( 'NONE', #8709, #14890, #4913, .T. ) ;
#7933 = ORIENTED_EDGE ( 'NONE', *, *, #282, .F. ) ;
#7934 = DIRECTION ( 'NONE',  ( 0.2872152572324145892, 0.9578660637129379207, -3.420201433256678811E-16 ) ) ;
#7935 = ORIENTED_EDGE ( 'NONE', *, *, #5360, .T. ) ;
#7936 = CARTESIAN_POINT ( 'NONE',  ( -7.768926039458051491, -39.58069824233449907, -0.5710089850524957544 ) ) ;
#7937 = DIRECTION ( 'NONE',  ( 8.018662683283438208E-16, -5.975035461963189015E-16, -1.000000000000000000 ) ) ;
#7938 = EDGE_CURVE ( 'NONE', #9010, #33, #12805, .T. ) ;
#7939 = DIRECTION ( 'NONE',  ( 0.5975035461963189576, 0.8018662683283437342, 0.000000000000000000 ) ) ;
#7940 = CARTESIAN_POINT ( 'NONE',  ( -8.885174762611967481, -49.00716318639572222, 44.32840209439113721 ) ) ;
#7941 = CARTESIAN_POINT ( 'NONE',  ( -6.534518714218351398, -9.065620043482315538, 60.62497794784820826 ) ) ;
#7942 = PLANE ( 'NONE',  #12872 ) ;
#7943 = EDGE_CURVE ( 'NONE', #10539, #3880, #9652, .T. ) ;
#7944 = DIRECTION ( 'NONE',  ( 8.018662683283438208E-16, -5.975035461963189015E-16, -1.000000000000000000 ) ) ;
#7945 = DIRECTION ( 'NONE',  ( -0.9225966037272106401, 0.3857661296576155863, -9.702957262759965065E-16 ) ) ;
#7946 = VERTEX_POINT ( 'NONE', #6039 ) ;
#7947 = CARTESIAN_POINT ( 'NONE',  ( 16.67206586382257072, -30.25228346699919868, 43.48069578308454908 ) ) ;
#7948 = ORIENTED_EDGE ( 'NONE', *, *, #14764, .T. ) ;
#7949 = DIRECTION ( 'NONE',  ( 0.2301973227387160703, -0.9731439732146149879, 7.660444431189776467E-16 ) ) ;
#7951 = ORIENTED_EDGE ( 'NONE', *, *, #3648, .F. ) ;
#7950 = FACE_OUTER_BOUND ( 'NONE', #9305, .T. ) ;
#7952 = EDGE_LOOP ( 'NONE', ( #9292, #2381, #6622, #6298 ) ) ;
#7953 = FACE_OUTER_BOUND ( 'NONE', #4072, .T. ) ;
#7954 = ORIENTED_EDGE ( 'NONE', *, *, #9317, .T. ) ;
#7955 = FACE_OUTER_BOUND ( 'NONE', #9789, .T. ) ;
#7956 = PRODUCT_RELATED_PRODUCT_CATEGORY ( 'part', '', ( #2011 ) ) ;
#7957 = EDGE_CURVE ( 'NONE', #11664, #3186, #4687, .T. ) ;
#7958 = CARTESIAN_POINT ( 'NONE',  ( -9.989347722329673829, -46.50737899243799944, -5.497689735156000346 ) ) ;
#7959 = EDGE_LOOP ( 'NONE', ( #488, #14806, #11131, #2857 ) ) ;
#7960 = CARTESIAN_POINT ( 'NONE',  ( -15.49969986081099904, -27.00737899243800300, -5.497689735156002122 ) ) ;
#7961 = ORIENTED_EDGE ( 'NONE', *, *, #10998, .T. ) ;
#7962 = CARTESIAN_POINT ( 'NONE',  ( 14.82713286944436781, -25.88435658361797564, 46.26984121431809172 ) ) ;
#7963 = EDGE_LOOP ( 'NONE', ( #12052, #1681, #721, #13717 ) ) ;
#7964 = DIRECTION ( 'NONE',  ( -0.3857661296576155308, -0.9225966037272105291, 2.419218955996680478E-16 ) ) ;
#7965 = ORIENTED_EDGE ( 'NONE', *, *, #5145, .T. ) ;
#7966 = EDGE_LOOP ( 'NONE', ( #1752, #7979, #8241, #14734, #1552 ) ) ;
#7967 = DIRECTION ( 'NONE',  ( 1.000000000000000000, 1.201369187114119994E-15, 9.616040805000176517E-16 ) ) ;
#7968 = EDGE_LOOP ( 'NONE', ( #8239, #4923, #7234, #7961 ) ) ;
#7969 = CARTESIAN_POINT ( 'NONE',  ( -15.36741682587554969, -22.58172476492607572, 56.85231026484400019 ) ) ;
#7970 = AXIS2_PLACEMENT_3D ( 'NONE', #11000, #9705, #8774 ) ;
#7971 = EDGE_CURVE ( 'NONE', #4831, #1003, #14321, .T. ) ;
#7972 = ADVANCED_FACE ( 'NONE', ( #2392 ), #250, .F. ) ;
#7973 = FACE_OUTER_BOUND ( 'NONE', #1833, .T. ) ;
#7974 = CARTESIAN_POINT ( 'NONE',  ( 4.185908152463202470, 11.99262100756819827, 16.16206422150100153 ) ) ;
#7975 = CIRCLE ( 'NONE', #6502, 10.00000000000000000 ) ;
#7976 = DIRECTION ( 'NONE',  ( -1.000000000000000000, 0.000000000000000000, 0.000000000000000000 ) ) ;
#7978 = CARTESIAN_POINT ( 'NONE',  ( 6.018379519091470620, 5.443421374437837024, 28.85885509741335753 ) ) ;
#7977 = DIRECTION ( 'NONE',  ( 1.000000000000000000, -1.291538348938060198E-32, 1.054621095516909827E-16 ) ) ;
#7979 = ORIENTED_EDGE ( 'NONE', *, *, #847, .T. ) ;
#7980 = DIRECTION ( 'NONE',  ( -0.7511640317997414495, -0.6601155939154573771, -2.079116908177570050E-16 ) ) ;
#7981 = AXIS2_PLACEMENT_3D ( 'NONE', #6402, #14529, #10147 ) ;
#7982 = CARTESIAN_POINT ( 'NONE',  ( -19.76919792506910412, -14.95941792723064090, -13.04426848743355549 ) ) ;
#7983 = EDGE_LOOP ( 'NONE', ( #108, #14435, #3081, #344 ) ) ;
#7984 = ORIENTED_EDGE ( 'NONE', *, *, #12738, .T. ) ;
#7985 = CARTESIAN_POINT ( 'NONE',  ( -15.49969986081092266, -109.4443699603185109, -0.1262635860074601546 ) ) ;
#7986 = VECTOR ( 'NONE', #3650, 1000.000000000000000 ) ;
#7987 = CARTESIAN_POINT ( 'NONE',  ( -22.78937479645117392, -41.20153274115700270, -17.28248307391377736 ) ) ;
#7988 = LINE ( 'NONE', #13896, #599 ) ;
#7989 = ORIENTED_EDGE ( 'NONE', *, *, #14873, .T. ) ;
#7990 = CARTESIAN_POINT ( 'NONE',  ( -15.16333526000375187, -10.64029123852186132, 56.75231026484397745 ) ) ;
#7991 = EDGE_CURVE ( 'NONE', #3619, #2590, #2465, .T. ) ;
#7992 = CARTESIAN_POINT ( 'NONE',  ( -3.508527451664998686, -47.37340439622244048, -3.997689735156000790 ) ) ;
#7993 = VECTOR ( 'NONE', #13168, 999.9999999999998863 ) ;
#7994 = CIRCLE ( 'NONE', #924, 9.974999999999999645 ) ;
#7995 = ITEM_DEFINED_TRANSFORMATION ( 'NONE', 'NONE', #3645,  #6789 ) ;
#7996 = CARTESIAN_POINT ( 'NONE',  ( -7.513186133687156598, -48.97671528745461700, 19.98830884321294832 ) ) ;
#7997 = VECTOR ( 'NONE', #10049, 1000.000000000000000 ) ;
#7998 = LINE ( 'NONE', #2200, #10148 ) ;
#7999 = CARTESIAN_POINT ( 'NONE',  ( -28.78282149594069850, -32.00737899243799944, 59.28069236156870403 ) ) ;
#8000 = VERTEX_POINT ( 'NONE', #2317 ) ;
#8001 = CARTESIAN_POINT ( 'NONE',  ( -12.20226299988479646, -91.14247851622610597, -1.229095371057126629 ) ) ;
#8002 = CARTESIAN_POINT ( 'NONE',  ( -34.10510093996977332, 6.837078596115874873, 30.39460083794530121 ) ) ;
#8003 = CARTESIAN_POINT ( 'NONE',  ( -18.09969986081099336, -109.6731500378498794, -10.30222923886191388 ) ) ;
#8004 = LINE ( 'NONE', #12693, #1446 ) ;
#8005 = VERTEX_POINT ( 'NONE', #11792 ) ;
#8006 = CIRCLE ( 'NONE', #10697, 8.000000000000000000 ) ;
#8007 = DIRECTION ( 'NONE',  ( 0.000000000000000000, -1.000000000000000000, -1.224646799147350002E-16 ) ) ;
#8008 = ORIENTED_EDGE ( 'NONE', *, *, #8188, .F. ) ;
#8009 = AXIS2_PLACEMENT_3D ( 'NONE', #1133, #10622, #9399 ) ;
#8010 = CARTESIAN_POINT ( 'NONE',  ( -21.45979773411919922, -21.50599501901345434, 54.00231026484399166 ) ) ;
#8011 = CARTESIAN_POINT ( 'NONE',  ( -15.49969986081100082, -109.7672458301522624, -0.6102019518851511393 ) ) ;
#8012 = EDGE_CURVE ( 'NONE', #6877, #9544, #9498, .T. ) ;
#8013 = CARTESIAN_POINT ( 'NONE',  ( -21.24026693782044717, -7.828337292084670551, 57.00231026484397745 ) ) ;
#8014 = CARTESIAN_POINT ( 'NONE',  ( -7.768926039458050603, -39.58069824233449907, 14.57562951474049129 ) ) ;
#8015 = AXIS2_PLACEMENT_3D ( 'NONE', #12895, #4705, #4781 ) ;
#8016 = EDGE_CURVE ( 'NONE', #3237, #1870, #3688, .T. ) ;
#8017 = DIRECTION ( 'NONE',  ( -1.000000000000000000, 0.000000000000000000, 0.000000000000000000 ) ) ;
#8018 = CARTESIAN_POINT ( 'NONE',  ( -15.49969986081099904, -44.50737899243799944, -109.5506571639849938 ) ) ;
#8019 = VECTOR ( 'NONE', #6973, 1000.000000000000000 ) ;
#8020 = LINE ( 'NONE', #5731, #14615 ) ;
#8021 = ADVANCED_FACE ( 'NONE', ( #14247 ), #3764, .T. ) ;
#8022 = DIRECTION ( 'NONE',  ( 0.000000000000000000, 0.1872998510044759646, 0.9823027872370621028 ) ) ;
#8023 = EDGE_LOOP ( 'NONE', ( #9885, #12829, #8432, #575 ) ) ;
#8024 = DIRECTION ( 'NONE',  ( 0.000000000000000000, 0.000000000000000000, -1.000000000000000000 ) ) ;
#8025 = VECTOR ( 'NONE', #3352, 1000.000000000000000 ) ;
#8027 = ORIENTED_EDGE ( 'NONE', *, *, #4800, .F. ) ;
#8026 = LINE ( 'NONE', #14, #6898 ) ;
#8028 = ORIENTED_EDGE ( 'NONE', *, *, #6046, .F. ) ;
#8029 = ORIENTED_EDGE ( 'NONE', *, *, #5788, .T. ) ;
#8030 = CARTESIAN_POINT ( 'NONE',  ( -16.10498554648963321, -110.4569083701214964, -10.53674001160706908 ) ) ;
#8031 = CARTESIAN_POINT ( 'NONE',  ( -15.49969986081092088, -13.50737899243822504, 56.85231026484398598 ) ) ;
#8032 = EDGE_LOOP ( 'NONE', ( #6125, #6091, #5583, #4332 ) ) ;
#8033 = DIRECTION ( 'NONE',  ( 0.000000000000000000, 1.000000000000000000, 1.224646799147350002E-16 ) ) ;
#8034 = EDGE_CURVE ( 'NONE', #5981, #5306, #14544, .T. ) ;
#8035 = EDGE_CURVE ( 'NONE', #7250, #10194, #6344, .T. ) ;
#8036 = CARTESIAN_POINT ( 'NONE',  ( -12.84086554789186607, -5.882298658668338120, 56.85231026484398598 ) ) ;
#8037 = CIRCLE ( 'NONE', #4140, 37.50000000000000000 ) ;
#8038 = VECTOR ( 'NONE', #58, 1000.000000000000000 ) ;
#8039 = VERTEX_POINT ( 'NONE', #4061 ) ;
#8040 = PLANE ( 'NONE',  #2764 ) ;
#8041 = ORIENTED_EDGE ( 'NONE', *, *, #11773, .F. ) ;
#8042 = CARTESIAN_POINT ( 'NONE',  ( -10.99969986081100259, -13.80113588252518397, -13.01695671647156338 ) ) ;
#8043 = ORIENTED_EDGE ( 'NONE', *, *, #9667, .T. ) ;
#8044 = CARTESIAN_POINT ( 'NONE',  ( -19.45253106704483770, -6.466019006254929202, 56.85231026484398598 ) ) ;
#8045 = ORIENTED_EDGE ( 'NONE', *, *, #7126, .F. ) ;
#8046 = ORIENTED_EDGE ( 'NONE', *, *, #9157, .F. ) ;
#8047 = CARTESIAN_POINT ( 'NONE',  ( -15.49969986081099904, 0.9926210075619987805, 24.21206422150099868 ) ) ;
#8048 = ORIENTED_EDGE ( 'NONE', *, *, #4995, .T. ) ;
#8049 = FACE_OUTER_BOUND ( 'NONE', #8183, .T. ) ;
#8050 = EDGE_CURVE ( 'NONE', #5847, #9327, #7578, .T. ) ;
#8051 = DIRECTION ( 'NONE',  ( 0.3633925226508256667, -0.9316361277244830097, 8.480480961564259036E-16 ) ) ;
#8052 = FACE_OUTER_BOUND ( 'NONE', #10655, .T. ) ;
#8053 = AXIS2_PLACEMENT_3D ( 'NONE', #14559, #494, #5148 ) ;
#8054 = CARTESIAN_POINT ( 'NONE',  ( -7.785174720008381399, -8.727488632615573394, 56.85231026484400019 ) ) ;
#8056 = DIRECTION ( 'NONE',  ( 0.000000000000000000, -1.000000000000000000, -1.224646799147350002E-16 ) ) ;
#8055 = DIRECTION ( 'NONE',  ( 0.5975035461963188466, 0.8018662683283437342, 0.000000000000000000 ) ) ;
#8057 = ORIENTED_EDGE ( 'NONE', *, *, #6921, .F. ) ;
#8058 = CARTESIAN_POINT ( 'NONE',  ( -7.499699860810997265, -44.62393082527479038, 42.84690782106163454 ) ) ;
#8059 = DIRECTION ( 'NONE',  ( -0.9826409426582665141, 0.1855175943453169496, -8.987940462991673516E-16 ) ) ;
#8060 = ORIENTED_EDGE ( 'NONE', *, *, #5276, .T. ) ;
#8061 = ORIENTED_EDGE ( 'NONE', *, *, #248, .F. ) ;
#8062 = FACE_OUTER_BOUND ( 'NONE', #7554, .T. ) ;
#8063 = EDGE_CURVE ( 'NONE', #8470, #2658, #14436, .T. ) ;
#8064 = VECTOR ( 'NONE', #1612, 1000.000000000000000 ) ;
#8065 = DIRECTION ( 'NONE',  ( 0.5975035461963189576, 0.8018662683283437342, 0.000000000000000000 ) ) ;
#8066 = CARTESIAN_POINT ( 'NONE',  ( -18.09969986081092586, -95.91433005893298969, -10.19792577984107318 ) ) ;
#8067 = ORIENTED_EDGE ( 'NONE', *, *, #10669, .F. ) ;
#8068 = DIRECTION ( 'NONE',  ( 0.9645173894937585368, 0.2640193276336892936, 6.156614753256587028E-16 ) ) ;
#8069 = FACE_OUTER_BOUND ( 'NONE', #4524, .T. ) ;
#8070 = CARTESIAN_POINT ( 'NONE',  ( -22.56723502526082470, -13.84084068328822248, 56.85231026484398598 ) ) ;
#8071 = DIRECTION ( 'NONE',  ( 0.000000000000000000, -0.1872998510044521503, -0.9823027872370667657 ) ) ;
#8072 = DIRECTION ( 'NONE',  ( 0.000000000000000000, 1.000000000000000000, 1.224646799147350002E-16 ) ) ;
#8073 = VERTEX_POINT ( 'NONE', #544 ) ;
#8074 = DIRECTION ( 'NONE',  ( -9.462935785116304784E-16, 0.9986295347545739443, -0.05233595624294359872 ) ) ;
#8075 = LINE ( 'NONE', #5785, #909 ) ;
#8076 = CARTESIAN_POINT ( 'NONE',  ( -17.95685260396766125, -23.17500669507537836, 57.00231026484399166 ) ) ;
#8077 = EDGE_CURVE ( 'NONE', #1607, #2329, #1487, .T. ) ;
#8078 = CARTESIAN_POINT ( 'NONE',  ( -21.17290370923395670, -9.280041403099277275, 57.00231026484397745 ) ) ;
#8079 = ORIENTED_EDGE ( 'NONE', *, *, #2874, .T. ) ;
#8080 = CARTESIAN_POINT ( 'NONE',  ( -7.595322498794511823, -45.75508878561614523, 46.89411779445664763 ) ) ;
#8081 = ORIENTED_EDGE ( 'NONE', *, *, #7255, .T. ) ;
#8082 = AXIS2_PLACEMENT_3D ( 'NONE', #6612, #9991, #10221 ) ;
#8083 = DIRECTION ( 'NONE',  ( 0.5975035461963188466, 0.8018662683283438453, 0.000000000000000000 ) ) ;
#8084 = DIRECTION ( 'NONE',  ( -0.5401126942952660936, -0.8415927028326163351, 6.975647374412055055E-17 ) ) ;
#8085 = FACE_OUTER_BOUND ( 'NONE', #3596, .T. ) ;
#8086 = CARTESIAN_POINT ( 'NONE',  ( -13.01672903104007872, -13.79867928167105440, 51.00231026484399166 ) ) ;
#8087 = CARTESIAN_POINT ( 'NONE',  ( -21.79367780933653620, -21.24601366423100401, 56.85231026484398598 ) ) ;
#8088 = VECTOR ( 'NONE', #1246, 1000.000000000000114 ) ;
#8089 = AXIS2_PLACEMENT_3D ( 'NONE', #1601, #6606, #13518 ) ;
#8090 = CARTESIAN_POINT ( 'NONE',  ( -20.65541546412893936, -22.04665423204160035, 57.00231026484397745 ) ) ;
#8091 = DIRECTION ( 'NONE',  ( 0.9183863840214729901, 0.3956847857120157075, 4.999999999999999402E-16 ) ) ;
#8092 = CARTESIAN_POINT ( 'NONE',  ( -13.18491133144367389, -15.23222315862922827, 51.00231026484399166 ) ) ;
#8093 = EDGE_CURVE ( 'NONE', #13514, #1150, #9537, .T. ) ;
#8094 = ORIENTED_EDGE ( 'NONE', *, *, #4203, .F. ) ;
#8095 = PLANE ( 'NONE',  #530 ) ;
#8096 = ORIENTED_EDGE ( 'NONE', *, *, #12608, .T. ) ;
#8097 = CARTESIAN_POINT ( 'NONE',  ( -24.85752488709640673, -10.05314452190415331, 56.85231026484398598 ) ) ;
#8099 = VERTEX_POINT ( 'NONE', #1840 ) ;
#8098 = CARTESIAN_POINT ( 'NONE',  ( -19.93511768254584027, -4.540527604665721917, 61.44996334348378753 ) ) ;
#8100 = VERTEX_POINT ( 'NONE', #3912 ) ;
#8101 = DIRECTION ( 'NONE',  ( -0.9826409426582659590, 0.1855175943453191978, -8.987940462991681405E-16 ) ) ;
#8102 = EDGE_CURVE ( 'NONE', #4677, #14676, #2913, .T. ) ;
#8103 = VECTOR ( 'NONE', #1192, 1000.000000000000000 ) ;
#8104 = FACE_OUTER_BOUND ( 'NONE', #2209, .T. ) ;
#8105 = ORIENTED_EDGE ( 'NONE', *, *, #4306, .T. ) ;
#8106 = AXIS2_PLACEMENT_3D ( 'NONE', #10240, #3208, #764 ) ;
#8107 = AXIS2_PLACEMENT_3D ( 'NONE', #11517, #5700, #10369 ) ;
#8108 = DIRECTION ( 'NONE',  ( 1.000000000000000000, 1.000000000000000078E-15, 0.000000000000000000 ) ) ;
#8109 = VECTOR ( 'NONE', #7857, 1000.000000000000000 ) ;
#8110 = DIRECTION ( 'NONE',  ( 0.4895147004624045839, -0.8719950447285823580, 9.135454576426008610E-16 ) ) ;
#8111 = DIRECTION ( 'NONE',  ( 0.000000000000000000, 0.000000000000000000, 1.000000000000000000 ) ) ;
#8112 = ADVANCED_FACE ( 'NONE', ( #1763 ), #477, .F. ) ;
#8113 = CONICAL_SURFACE ( 'NONE', #2762, 2.000000000000001776, 0.7853981633974476129 ) ;
#8114 =( BOUNDED_CURVE ( )  B_SPLINE_CURVE ( 3, ( #6686, #10522, #971, #7985 ),
 .UNSPECIFIED., .F., .F. ) 
 B_SPLINE_CURVE_WITH_KNOTS ( ( 4, 4 ),
 ( 4.712388980384689674, 6.283185307179586232 ),
 .UNSPECIFIED. ) 
 CURVE ( )  GEOMETRIC_REPRESENTATION_ITEM ( )  RATIONAL_B_SPLINE_CURVE ( ( 1.000000000000000000, 0.8047378541243649375, 0.8047378541243649375, 1.000000000000000000 ) ) 
 REPRESENTATION_ITEM ( '' )  );
#8115 = CARTESIAN_POINT ( 'NONE',  ( -17.58173612995575397, -52.24942676811487274, -17.94337340107023593 ) ) ;
#8116 = EDGE_CURVE ( 'NONE', #13227, #14849, #6268, .T. ) ;
#8117 = ORIENTED_EDGE ( 'NONE', *, *, #5334, .T. ) ;
#8118 = CARTESIAN_POINT ( 'NONE',  ( -15.20596105127630082, -18.00737899243800655, -13.28793577849899599 ) ) ;
#8119 = EDGE_CURVE ( 'NONE', #14475, #11680, #9798, .T. ) ;
#8120 = ORIENTED_EDGE ( 'NONE', *, *, #2797, .F. ) ;
#8121 = DIRECTION ( 'NONE',  ( 0.5975035461963188466, 0.8018662683283437342, 0.000000000000000000 ) ) ;
#8122 = ORIENTED_EDGE ( 'NONE', *, *, #14522, .T. ) ;
#8123 = VERTEX_POINT ( 'NONE', #7343 ) ;
#8124 = EDGE_CURVE ( 'NONE', #9649, #1625, #11899, .T. ) ;
#8125 = CARTESIAN_POINT ( 'NONE',  ( 3.100272115295338970, -39.60750234070978593, 52.06484617642751545 ) ) ;
#8126 = EDGE_LOOP ( 'NONE', ( #4700, #14737, #8644, #14639 ) ) ;
#8127 = CARTESIAN_POINT ( 'NONE',  ( -7.528759897616733809, -14.80173833325270571, 56.85231026484400019 ) ) ;
#8128 = EDGE_CURVE ( 'NONE', #3162, #1870, #5534, .T. ) ;
#8129 = AXIS2_PLACEMENT_3D ( 'NONE', #9022, #8944, #5732 ) ;
#8130 = CARTESIAN_POINT ( 'NONE',  ( 0.8003001391889992266, 11.99262100756199878, 24.16206422150099442 ) ) ;
#8131 = CARTESIAN_POINT ( 'NONE',  ( -9.760873592531984499, -5.348549538251087476, 54.00231026484399166 ) ) ;
#8132 = AXIS2_PLACEMENT_3D ( 'NONE', #9688, #13147, #10911 ) ;
#8133 = CARTESIAN_POINT ( 'NONE',  ( -7.508851067721073136, -44.91495161711613804, 21.42953195777254294 ) ) ;
#8135 = LINE ( 'NONE', #10516, #12682 ) ;
#8134 = CARTESIAN_POINT ( 'NONE',  ( -24.08903783298838519, -16.43731469134198520, 57.00231026484397745 ) ) ;
#8136 = ORIENTED_EDGE ( 'NONE', *, *, #8594, .F. ) ;
#8137 = PLANE ( 'NONE',  #15095 ) ;
#8138 = EDGE_CURVE ( 'NONE', #532, #7723, #10915, .T. ) ;
#8139 = EDGE_CURVE ( 'NONE', #2792, #4546, #2987, .T. ) ;
#8140 = FACE_OUTER_BOUND ( 'NONE', #2778, .T. ) ;
#8141 = ORIENTED_EDGE ( 'NONE', *, *, #10463, .F. ) ;
#8142 = ORIENTED_EDGE ( 'NONE', *, *, #5854, .F. ) ;
#8143 = FACE_OUTER_BOUND ( 'NONE', #776, .T. ) ;
#8144 = VECTOR ( 'NONE', #14371, 999.9999999999998863 ) ;
#8145 = CARTESIAN_POINT ( 'NONE',  ( -23.48648741169278864, -43.97817952596684421, 56.14193264201148992 ) ) ;
#8146 = ORIENTED_EDGE ( 'NONE', *, *, #14356, .F. ) ;
#8147 = CARTESIAN_POINT ( 'NONE',  ( -7.771455047768278668, -42.42330350419953788, -17.19278996553040528 ) ) ;
#8148 = EDGE_LOOP ( 'NONE', ( #12489, #14777, #12496, #12792 ) ) ;
#8149 = VECTOR ( 'NONE', #10387, 1000.000000000000227 ) ;
#8150 = CARTESIAN_POINT ( 'NONE',  ( -20.19618812003464470, -21.27295997720514720, 56.85231026484398598 ) ) ;
#8151 = CONTEXT_DEPENDENT_SHAPE_REPRESENTATION ( #11335, #7492 ) ;
#8152 = EDGE_CURVE ( 'NONE', #11125, #3375, #10878, .T. ) ;
#8153 = VECTOR ( 'NONE', #5293, 1000.000000000000000 ) ;
#8154 = DIRECTION ( 'NONE',  ( -1.054621095516909827E-16, -1.224646799147350002E-16, 1.000000000000000000 ) ) ;
#8155 = CARTESIAN_POINT ( 'NONE',  ( -13.72291223624743317, -3.691898834178107602, 57.00231026484397745 ) ) ;
#8156 = CARTESIAN_POINT ( 'NONE',  ( -7.285742840713465007, -17.36641515085804599, 57.00231026484399166 ) ) ;
#8157 = ORIENTED_EDGE ( 'NONE', *, *, #12103, .F. ) ;
#8158 = CARTESIAN_POINT ( 'NONE',  ( -12.57554303975000742, -91.34342846084412315, -0.9737555918262782439 ) ) ;
#8159 = CARTESIAN_POINT ( 'NONE',  ( -17.81448839017816965, -11.78253482624722004, 56.75231026484397745 ) ) ;
#8160 = CIRCLE ( 'NONE', #10109, 2.500000000000000444 ) ;
#8161 = CARTESIAN_POINT ( 'NONE',  ( -18.09969986081099336, -109.6015874540538846, -10.30597967495842227 ) ) ;
#8162 = LINE ( 'NONE', #7649, #230 ) ;
#8163 = ORIENTED_EDGE ( 'NONE', *, *, #619, .T. ) ;
#8164 = CARTESIAN_POINT ( 'NONE',  ( -17.72867398697626129, -22.30470383268854562, 56.85231026484400019 ) ) ;
#8165 = ORIENTED_EDGE ( 'NONE', *, *, #11051, .T. ) ;
#8166 = CARTESIAN_POINT ( 'NONE',  ( -7.499849062438288527, -12.40572695854698360, 56.85231026484400019 ) ) ;
#8167 = LINE ( 'NONE', #12856, #3383 ) ;
#8168 = CARTESIAN_POINT ( 'NONE',  ( -9.291286065451622278, -6.887949398765353060, 56.85231026484398598 ) ) ;
#8169 = CARTESIAN_POINT ( 'NONE',  ( -18.48721759179251123, -17.51671033407994926, 54.00231026484399166 ) ) ;
#8170 = EDGE_CURVE ( 'NONE', #11942, #9206, #10031, .T. ) ;
#8171 = CARTESIAN_POINT ( 'NONE',  ( -15.49969986081098838, -17.75737899243799944, 51.00231026484400587 ) ) ;
#8172 = CIRCLE ( 'NONE', #13080, 2.500000000000000444 ) ;
#8173 = DIRECTION ( 'NONE',  ( 8.018662683283438208E-16, -5.975035461963189015E-16, -1.000000000000000000 ) ) ;
#8174 = CARTESIAN_POINT ( 'NONE',  ( -13.92794721577312878, -5.586467200048621073, 56.85231026484398598 ) ) ;
#8175 = CARTESIAN_POINT ( 'NONE',  ( -36.79886583278639023, -37.30547240248171903, 50.36646496601539980 ) ) ;
#8176 = DIRECTION ( 'NONE',  ( -0.9040177279761104634, -0.4274949678123838859, -4.694715627858909121E-16 ) ) ;
#8177 = VERTEX_POINT ( 'NONE', #4367 ) ;
#8178 = DIRECTION ( 'NONE',  ( 0.5975035461963189576, 0.8018662683283437342, 0.000000000000000000 ) ) ;
#8179 = PRODUCT_DEFINITION_CONTEXT ( 'detailed design', #14753, 'design' ) ;
#8180 = EDGE_LOOP ( 'NONE', ( #7850, #1775, #8480, #10672 ) ) ;
#8182 = EDGE_LOOP ( 'NONE', ( #247, #10295, #7137, #7948 ) ) ;
#8181 = DIRECTION ( 'NONE',  ( -1.000000000000000078E-15, 1.000000000000000000, 0.000000000000000000 ) ) ;
#8183 = EDGE_LOOP ( 'NONE', ( #5697, #2840, #9678, #13600 ) ) ;
#8184 = PLANE ( 'NONE',  #10685 ) ;
#8185 = ORIENTED_EDGE ( 'NONE', *, *, #10616, .F. ) ;
#8186 = DIRECTION ( 'NONE',  ( -1.000000000000000472E-15, 0.9823027872370664326, -0.1872998510044540932 ) ) ;
#8187 = CARTESIAN_POINT ( 'NONE',  ( -20.87112600995946110, -107.9638125199853533, -5.349927266640145618 ) ) ;
#8188 = EDGE_CURVE ( 'NONE', #1150, #13514, #5300, .T. ) ;
#8189 = DIRECTION ( 'NONE',  ( 8.018662683283438208E-16, -5.975035461963189015E-16, -1.000000000000000000 ) ) ;
#8190 = DIRECTION ( 'NONE',  ( 0.000000000000000000, 0.000000000000000000, 1.000000000000000000 ) ) ;
#8191 = CARTESIAN_POINT ( 'NONE',  ( -19.85426396466228027, -12.33449077490513623, -13.03429394648231643 ) ) ;
#8192 = EDGE_CURVE ( 'NONE', #2509, #9604, #10246, .T. ) ;
#8193 = DIRECTION ( 'NONE',  ( 1.000000000000000078E-15, -1.000000000000000000, 0.000000000000000000 ) ) ;
#8194 = LINE ( 'NONE', #10803, #14969 ) ;
#8195 = ORIENTED_EDGE ( 'NONE', *, *, #11717, .F. ) ;
#8196 = CARTESIAN_POINT ( 'NONE',  ( 3.112640221700739840, -39.60748137431547633, -13.05276465491907345 ) ) ;
#8197 = ORIENTED_EDGE ( 'NONE', *, *, #849, .F. ) ;
#8198 = AXIS2_PLACEMENT_3D ( 'NONE', #1755, #9795, #5273 ) ;
#8199 = FACE_OUTER_BOUND ( 'NONE', #7354, .T. ) ;
#8200 = ORIENTED_EDGE ( 'NONE', *, *, #5275, .T. ) ;
#8201 = ORIENTED_EDGE ( 'NONE', *, *, #6061, .T. ) ;
#8202 = DIRECTION ( 'NONE',  ( -8.018662683283438208E-16, 5.975035461963189015E-16, 1.000000000000000000 ) ) ;
#8203 = ORIENTED_EDGE ( 'NONE', *, *, #1293, .T. ) ;
#8204 = FACE_OUTER_BOUND ( 'NONE', #54, .T. ) ;
#8205 = EDGE_CURVE ( 'NONE', #10768, #5054, #10161, .T. ) ;
#8206 = DIRECTION ( 'NONE',  ( 0.000000000000000000, -1.000000000000000000, -1.224646799147350002E-16 ) ) ;
#8207 = DIRECTION ( 'NONE',  ( -0.9918751611018171710, -0.1272150336605075427, -7.193398003386516820E-16 ) ) ;
#8208 = CIRCLE ( 'NONE', #2360, 9.974999999999999645 ) ;
#8209 = EDGE_CURVE ( 'NONE', #9803, #7103, #14584, .T. ) ;
#8210 = PLANE ( 'NONE',  #122 ) ;
#8212 = CARTESIAN_POINT ( 'NONE',  ( -34.99969986081099904, -19.50737899243800300, -17.99768973515599768 ) ) ;
#8211 = DIRECTION ( 'NONE',  ( -0.9437508163134049610, -0.3306575217771128283, -5.591929034707468788E-16 ) ) ;
#8213 = ORIENTED_EDGE ( 'NONE', *, *, #13794, .T. ) ;
#8214 = DIRECTION ( 'NONE',  ( -0.9547156899063192759, -0.2975196656469966672, -5.877852522924767272E-16 ) ) ;
#8215 = CARTESIAN_POINT ( 'NONE',  ( -10.12676381431746542, -90.53940471697117687, -5.497640657892870486 ) ) ;
#8216 = VERTEX_POINT ( 'NONE', #12706 ) ;
#8217 = EDGE_CURVE ( 'NONE', #4500, #1475, #4518, .T. ) ;
#8218 = ORIENTED_EDGE ( 'NONE', *, *, #10942, .F. ) ;
#8219 = CARTESIAN_POINT ( 'NONE',  ( 21.85920135429435263, -27.00737899243800300, 27.46206422150099868 ) ) ;
#8220 = CARTESIAN_POINT ( 'NONE',  ( -16.54355812366951284, -36.55815850481217666, 56.99137402710550049 ) ) ;
#8221 = VECTOR ( 'NONE', #4118, 1000.000000000000227 ) ;
#8222 = VERTEX_POINT ( 'NONE', #2219 ) ;
#8223 = CARTESIAN_POINT ( 'NONE',  ( -8.013558459183959926, -41.67444402531860703, -17.24300375686068421 ) ) ;
#8224 = EDGE_LOOP ( 'NONE', ( #14997, #4237, #14793, #13788 ) ) ;
#8225 = CONICAL_SURFACE ( 'NONE', #1399, 6.000000000000001776, 0.03490658503988566114 ) ;
#8226 = EDGE_CURVE ( 'NONE', #9490, #6457, #9095, .T. ) ;
#8227 = FACE_OUTER_BOUND ( 'NONE', #10327, .T. ) ;
#8228 = EDGE_CURVE ( 'NONE', #1568, #11735, #7789, .T. ) ;
#8229 = VECTOR ( 'NONE', #8308, 1000.000000000000000 ) ;
#8230 = CARTESIAN_POINT ( 'NONE',  ( -1.508527451665001351, -45.20834088676132723, -4.747689735156000346 ) ) ;
#8231 = CIRCLE ( 'NONE', #10440, 3.249999999999999556 ) ;
#8232 = CARTESIAN_POINT ( 'NONE',  ( -18.09969986081100046, -109.6217528783177784, -2.009566970250350693 ) ) ;
#8233 = LINE ( 'NONE', #7999, #13550 ) ;
#8234 = ORIENTED_EDGE ( 'NONE', *, *, #1574, .F. ) ;
#8235 = DIRECTION ( 'NONE',  ( 3.632077277826439854E-16, -1.000000000000000000, 0.000000000000000000 ) ) ;
#8236 = CARTESIAN_POINT ( 'NONE',  ( -24.01584079503567182, -10.37104457333969876, 56.85231026484398598 ) ) ;
#8237 = ORIENTED_EDGE ( 'NONE', *, *, #2692, .T. ) ;
#8238 = LINE ( 'NONE', #1584, #10980 ) ;
#8239 = ORIENTED_EDGE ( 'NONE', *, *, #3814, .T. ) ;
#8240 = DIRECTION ( 'NONE',  ( 0.000000000000000000, 0.1872998510044689147, 0.9823027872370635460 ) ) ;
#8241 = ORIENTED_EDGE ( 'NONE', *, *, #6368, .T. ) ;
#8242 = CARTESIAN_POINT ( 'NONE',  ( -5.499699860810998153, -46.50737899243799944, -8.497689735156003010 ) ) ;
#8243 = DIRECTION ( 'NONE',  ( 0.5975035461963189576, 0.8018662683283437342, 0.000000000000000000 ) ) ;
#8244 = AXIS2_PLACEMENT_3D ( 'NONE', #14602, #1829, #757 ) ;
#8245 = VECTOR ( 'NONE', #10380, 1000.000000000000000 ) ;
#8246 = CARTESIAN_POINT ( 'NONE',  ( -8.663330333365388825, -17.80566954616001496, 56.85231026484400019 ) ) ;
#8247 = CARTESIAN_POINT ( 'NONE',  ( -15.49969986081099194, -36.50737899243799944, 11.50231026484399699 ) ) ;
#8248 = DIRECTION ( 'NONE',  ( 1.000000000000000000, 0.000000000000000000, 0.000000000000000000 ) ) ;
#8249 = FACE_OUTER_BOUND ( 'NONE', #89, .T. ) ;
#8250 = FACE_OUTER_BOUND ( 'NONE', #14548, .T. ) ;
#8251 = LINE ( 'NONE', #13925, #11433 ) ;
#8252 = CARTESIAN_POINT ( 'NONE',  ( -17.40065610530428586, -5.145404622917534532, 56.85231026484398598 ) ) ;
#8253 = AXIS2_PLACEMENT_3D ( 'NONE', #13841, #9165, #1986 ) ;
#8254 = VERTEX_POINT ( 'NONE', #3293 ) ;
#8255 = CARTESIAN_POINT ( 'NONE',  ( -18.68395610307571530, -20.92841410781112899, 56.85231026484398598 ) ) ;
#8256 = VERTEX_POINT ( 'NONE', #7862 ) ;
#8258 = ORIENTED_EDGE ( 'NONE', *, *, #2655, .T. ) ;
#8257 = CARTESIAN_POINT ( 'NONE',  ( -18.09969986081100402, -105.5768790231641248, -6.170773065691671277 ) ) ;
#8259 = ORIENTED_EDGE ( 'NONE', *, *, #12178, .T. ) ;
#8260 = EDGE_CURVE ( 'NONE', #11198, #3205, #11249, .T. ) ;
#8261 = CARTESIAN_POINT ( 'NONE',  ( -18.54556661251663385, -20.98627902725976568, 57.00231026484397745 ) ) ;
#8262 = ORIENTED_EDGE ( 'NONE', *, *, #12043, .F. ) ;
#8263 = VECTOR ( 'NONE', #13731, 1000.000000000000114 ) ;
#8264 = LINE ( 'NONE', #12957, #13808 ) ;
#8265 = AXIS2_PLACEMENT_3D ( 'NONE', #5327, #4335, #7685 ) ;
#8266 = DIRECTION ( 'NONE',  ( 0.9983330752162417054, 0.05771543059946734194, 7.660444431189781397E-16 ) ) ;
#8267 = DIRECTION ( 'NONE',  ( 0.5975035461963189576, 0.8018662683283437342, 0.000000000000000000 ) ) ;
#8268 = DIRECTION ( 'NONE',  ( 9.943800201373337757E-16, -0.1872998510044509290, -0.9823027872370669877 ) ) ;
#8269 = CARTESIAN_POINT ( 'NONE',  ( -7.499699860810999041, -19.50737899243799589, 54.00231026484400587 ) ) ;
#8270 = FACE_OUTER_BOUND ( 'NONE', #7796, .T. ) ;
#8271 = CARTESIAN_POINT ( 'NONE',  ( 5.901818273210405863, -37.26927769664150958, -11.29100291904106612 ) ) ;
#8272 = ORIENTED_EDGE ( 'NONE', *, *, #13938, .F. ) ;
#8273 = ORIENTED_EDGE ( 'NONE', *, *, #5415, .T. ) ;
#8274 = ORIENTED_EDGE ( 'NONE', *, *, #3359, .F. ) ;
#8275 = CARTESIAN_POINT ( 'NONE',  ( -22.53804163936502647, -6.438972523632135569, 56.85231026484398598 ) ) ;
#8276 = EDGE_CURVE ( 'NONE', #645, #1981, #5060, .T. ) ;
#8277 = CLOSED_SHELL ( 'NONE', ( #1288, #1873, #7207, #1034, #2296, #8382, #11476, #3152, #11030, #1916, #829, #13769, #10196, #9425, #13848, #758, #13370, #10480, #2102, #12541, #15101, #10283, #14219, #11122, #11317, #11766, #8662, #1915, #8302, #6616, #11844, #4981, #10107, #1707, #8414, #653, #14010, #8863, #10048, #10751, #1972, #10401, #7786, #8021, #3865, #13039, #955, #3850, #6324, #12349, #5756, #2624, #4876, #10834, #11431, #12061, #9771, #11600, #5872, #2087, #13211, #5969, #4264, #5834, #4472, #2900, #9105, #14211, #5669, #12341, #9993, #1035, #2467, #1304, #1846, #8401, #1360, #9788, #13493, #6935, #10121, #15000, #11971, #12446, #3174, #2420, #10004, #2270, #10157, #11012, #3363, #1766, #11583, #11211, #10264, #9722, #4158, #12437, #132, #3586, #11794, #14373, #1861, #10073, #14558, #7005, #6883, #7497, #4282, #10375, #3767, #6468, #6303, #5099, #7695, #13654, #11604, #4665, #284, #2726, #12538, #3207, #12354, #10511, #4299, #5243, #2436, #14656, #3449, #9228, #8571, #4971, #1269, #6199, #12736, #7731, #13805, #7084, #7515, #3418, #8510, #13869, #5484, #13208, #833, #10154, #3550, #10949, #12064, #14680, #6786, #5709, #9267, #7414, #3553, #4493, #11132, #12592, #11208, #14509, #14946, #10881, #6234, #6149, #12765, #14323, #473, #13621, #11227, #6807, #11518, #1757, #3725, #6713, #3400, #12723, #1214, #13831, #8985, #25, #2207, #2499, #635, #13766, #7516, #14618, #12216, #11390, #4026, #9905, #15123, #3554, #13019, #2239, #4474, #13506, #13355, #9336, #6765, #2426, #7313, #1181, #6130, #7633, #9654, #10740, #1448, #11989, #11783, #1347, #4368, #7466, #3924, #7604, #7775, #14069, #13919, #6075 ) ) ;
#8278 = CARTESIAN_POINT ( 'NONE',  ( 4.144397788355465018, -38.30087877078349834, 51.44538043376633141 ) ) ;
#8279 = ORIENTED_EDGE ( 'NONE', *, *, #5430, .F. ) ;
#8280 = CARTESIAN_POINT ( 'NONE',  ( -15.49969986081099904, 4.873818854045000037, 24.21206422150099868 ) ) ;
#8281 = CIRCLE ( 'NONE', #1691, 8.000000000000000000 ) ;
#8282 = AXIS2_PLACEMENT_3D ( 'NONE', #9147, #7837, #13824 ) ;
#8283 = CARTESIAN_POINT ( 'NONE',  ( 0.8003001391889992266, 20.99262100756200056, 16.16206422150100153 ) ) ;
#8284 = FACE_OUTER_BOUND ( 'NONE', #377, .T. ) ;
#8285 = DIRECTION ( 'NONE',  ( 0.3956847857120156520, -0.9183863840214728791, 8.660254037844387408E-16 ) ) ;
#8287 = CARTESIAN_POINT ( 'NONE',  ( -15.49969986081099904, 13.89262100756199736, 24.21206422150099868 ) ) ;
#8286 = CARTESIAN_POINT ( 'NONE',  ( -7.838594959941967311, -47.52544946159166983, -3.196372820239050228 ) ) ;
#8288 = EDGE_LOOP ( 'NONE', ( #13962, #9488 ) ) ;
#8289 = FACE_OUTER_BOUND ( 'NONE', #15112, .T. ) ;
#8290 = LINE ( 'NONE', #7139, #13767 ) ;
#8291 = VERTEX_POINT ( 'NONE', #12476 ) ;
#8292 = AXIS2_PLACEMENT_3D ( 'NONE', #8752, #7606, #1955 ) ;
#8293 = VERTEX_POINT ( 'NONE', #10323 ) ;
#8294 = ADVANCED_FACE ( 'NONE', ( #5428 ), #13620, .F. ) ;
#8295 = CARTESIAN_POINT ( 'NONE',  ( -19.04179444808664812, -37.32947002669901337, 56.83537356607605062 ) ) ;
#8296 = ORIENTED_EDGE ( 'NONE', *, *, #15055, .T. ) ;
#8297 = DIRECTION ( 'NONE',  ( 1.000000000000000000, 1.000000000000000078E-15, 0.000000000000000000 ) ) ;
#8298 = EDGE_CURVE ( 'NONE', #2388, #2863, #1070, .T. ) ;
#8299 = AXIS2_PLACEMENT_3D ( 'NONE', #9183, #9035, #14785 ) ;
#8300 = DIRECTION ( 'NONE',  ( -0.9547156899063178326, -0.2975196656470014966, -5.877852522924727828E-16 ) ) ;
#8301 = DIRECTION ( 'NONE',  ( -8.018662683283438208E-16, 5.975035461963189015E-16, 1.000000000000000000 ) ) ;
#8302 = ADVANCED_FACE ( 'NONE', ( #10089 ), #14689, .F. ) ;
#8303 = PLANE ( 'NONE',  #14319 ) ;
#8304 = PLANE ( 'NONE',  #7882 ) ;
#8306 = ORIENTED_EDGE ( 'NONE', *, *, #4402, .F. ) ;
#8305 = AXIS2_PLACEMENT_3D ( 'NONE', #12342, #1559, #5226 ) ;
#8307 = CARTESIAN_POINT ( 'NONE',  ( 2.377116011596429601, -23.18484177525208167, 57.27215087687874018 ) ) ;
#8308 = DIRECTION ( 'NONE',  ( -8.018662683283438208E-16, 5.975035461963189015E-16, 1.000000000000000000 ) ) ;
#8309 = ORIENTED_EDGE ( 'NONE', *, *, #6536, .T. ) ;
#8310 = ADVANCED_FACE ( 'NONE', ( #7711, #12941, #6937, #5950 ), #10476, .T. ) ;
#8312 = EDGE_CURVE ( 'NONE', #6022, #3165, #3744, .T. ) ;
#8311 = CARTESIAN_POINT ( 'NONE',  ( 9.000300139189000959, -27.00737899243800300, 21.71206422150100224 ) ) ;
#8313 = ORIENTED_EDGE ( 'NONE', *, *, #4404, .T. ) ;
#8314 = CARTESIAN_POINT ( 'NONE',  ( -20.69940085690220144, -18.30574950243923027, 56.85231026484398598 ) ) ;
#8315 = EDGE_LOOP ( 'NONE', ( #8273, #5879, #4554, #2687, #14422, #1768 ) ) ;
#8316 = DIRECTION ( 'NONE',  ( 0.5975035461963188466, 0.8018662683283437342, 0.000000000000000000 ) ) ;
#8317 = EDGE_CURVE ( 'NONE', #9206, #6888, #4035, .T. ) ;
#8318 = DIRECTION ( 'NONE',  ( -1.000000000000000078E-15, 1.000000000000000000, 0.000000000000000000 ) ) ;
#8319 = DIRECTION ( 'NONE',  ( 0.000000000000000000, 1.850371707708594316E-16, -1.000000000000000000 ) ) ;
#8320 = CARTESIAN_POINT ( 'NONE',  ( -24.80452494096261518, -9.912819877918103373, 54.00231026484397745 ) ) ;
#8321 = CARTESIAN_POINT ( 'NONE',  ( -15.49969986081099904, 13.89262100756199736, 24.21206422150099868 ) ) ;
#8322 = CARTESIAN_POINT ( 'NONE',  ( -8.722797460041883610, -15.53942693735753444, 56.85231026484400019 ) ) ;
#8323 = CARTESIAN_POINT ( 'NONE',  ( 14.82707475067032199, -28.13046415553212043, 2.154202982575026404 ) ) ;
#8324 = VERTEX_POINT ( 'NONE', #4820 ) ;
#8325 = CARTESIAN_POINT ( 'NONE',  ( -12.81093390292742740, -9.898980784960722090, -13.99768973515600301 ) ) ;
#8326 = CARTESIAN_POINT ( 'NONE',  ( -15.26225645643175710, -10.41069464251649279, 57.00231026484397745 ) ) ;
#8327 = VECTOR ( 'NONE', #7664, 1000.000000000000227 ) ;
#8328 = CARTESIAN_POINT ( 'NONE',  ( -17.61203582817000068, -107.1622034095870077, -6.087689735156001980 ) ) ;
#8329 = VERTEX_POINT ( 'NONE', #10626 ) ;
#8330 = CARTESIAN_POINT ( 'NONE',  ( -15.49969986081092088, -13.50737899243822504, 56.85231026484398598 ) ) ;
#8331 = UNCERTAINTY_MEASURE_WITH_UNIT (LENGTH_MEASURE( 1.000000000000000082E-05 ), #13863, 'distance_accuracy_value', 'NONE');
#8332 = ADVANCED_FACE ( 'NONE', ( #3 ), #232, .F. ) ;
#8333 = ORIENTED_EDGE ( 'NONE', *, *, #7957, .F. ) ;
#8335 = ORIENTED_EDGE ( 'NONE', *, *, #11880, .T. ) ;
#8334 = LINE ( 'NONE', #1228, #2280 ) ;
#8336 = ORIENTED_EDGE ( 'NONE', *, *, #4397, .F. ) ;
#8337 = DIRECTION ( 'NONE',  ( 0.000000000000000000, 0.05233595624294329340, 0.9986295347545738332 ) ) ;
#8338 = EDGE_CURVE ( 'NONE', #8291, #13071, #4590, .T. ) ;
#8339 = CARTESIAN_POINT ( 'NONE',  ( -19.68577560955674954, -20.41303028871448788, 56.85231026484398598 ) ) ;
#8340 = ORIENTED_EDGE ( 'NONE', *, *, #11548, .T. ) ;
#8341 = FACE_OUTER_BOUND ( 'NONE', #2441, .T. ) ;
#8342 = CARTESIAN_POINT ( 'NONE',  ( -12.52039621090187893, -4.935039769003430443, 57.00231026484397745 ) ) ;
#8343 = AXIS2_PLACEMENT_3D ( 'NONE', #9642, #2603, #14662 ) ;
#8344 = CARTESIAN_POINT ( 'NONE',  ( -12.38873450203231030, -7.152605626181999909, 57.00231026484397745 ) ) ;
#8345 = DIRECTION ( 'NONE',  ( 1.000000000000000000, 0.000000000000000000, 0.000000000000000000 ) ) ;
#8346 = CARTESIAN_POINT ( 'NONE',  ( 18.53245405280430091, -26.77391037161654808, 8.462064221500996908 ) ) ;
#8347 = EDGE_CURVE ( 'NONE', #221, #12795, #10547, .T. ) ;
#8348 = CARTESIAN_POINT ( 'NONE',  ( -8.681233859935401753, -6.226640953275941470, 57.00231026484397745 ) ) ;
#8349 = AXIS2_PLACEMENT_3D ( 'NONE', #4167, #3944, #8672 ) ;
#8350 = DIRECTION ( 'NONE',  ( 0.5975035461963188466, 0.8018662683283437342, 0.000000000000000000 ) ) ;
#8351 = VERTEX_POINT ( 'NONE', #5800 ) ;
#8352 = CARTESIAN_POINT ( 'NONE',  ( -15.49969986081092088, -13.50737899243822504, 56.85231026484398598 ) ) ;
#8353 = VERTEX_POINT ( 'NONE', #1138 ) ;
#8354 = ORIENTED_EDGE ( 'NONE', *, *, #3690, .T. ) ;
#8355 = VECTOR ( 'NONE', #5845, 1000.000000000000000 ) ;
#8356 = AXIS2_PLACEMENT_3D ( 'NONE', #1974, #8845, #10066 ) ;
#8357 = CARTESIAN_POINT ( 'NONE',  ( 5.737180257485530177, -37.32854632935037387, 50.40935528563701240 ) ) ;
#8358 = VERTEX_POINT ( 'NONE', #13086 ) ;
#8359 = LINE ( 'NONE', #13046, #13955 ) ;
#8360 = DIRECTION ( 'NONE',  ( 0.000000000000000000, 0.000000000000000000, 1.000000000000000000 ) ) ;
#8361 = DIRECTION ( 'NONE',  ( 0.08178736187251967049, 0.9966498018049938512, -5.299192642332049884E-16 ) ) ;
#8362 = EDGE_CURVE ( 'NONE', #5856, #4847, #11929, .T. ) ;
#8363 = AXIS2_PLACEMENT_3D ( 'NONE', #14467, #2770, #9944 ) ;
#8364 = FACE_OUTER_BOUND ( 'NONE', #6110, .T. ) ;
#8366 = CARTESIAN_POINT ( 'NONE',  ( -36.42585024326910315, 12.65779542994580353, 32.26206422150099939 ) ) ;
#8365 = CARTESIAN_POINT ( 'NONE',  ( -7.600774661674001287, -48.67202872725436436, -4.244403150344465026 ) ) ;
#8367 = ORIENTED_EDGE ( 'NONE', *, *, #2248, .T. ) ;
#8368 = CARTESIAN_POINT ( 'NONE',  ( -14.60940909295887913, -15.57374835648654532, 51.25231026484399166 ) ) ;
#8369 = DIRECTION ( 'NONE',  ( 0.000000000000000000, 0.000000000000000000, 1.000000000000000000 ) ) ;
#8370 = ORIENTED_EDGE ( 'NONE', *, *, #7681, .F. ) ;
#8371 = ORIENTED_EDGE ( 'NONE', *, *, #14054, .T. ) ;
#8372 = DIRECTION ( 'NONE',  ( -1.054621095516909827E-16, 1.224646799147350002E-16, -1.000000000000000000 ) ) ;
#8373 = EDGE_LOOP ( 'NONE', ( #10035, #12622 ) ) ;
#8374 = CARTESIAN_POINT ( 'NONE',  ( -9.145157332402543915, -39.61893914866874411, -17.45656333442792274 ) ) ;
#8375 = CIRCLE ( 'NONE', #7401, 0.4500000000000011768 ) ;
#8376 = CARTESIAN_POINT ( 'NONE',  ( -20.44787060326519423, -4.846187890544671362, 57.00231026484397745 ) ) ;
#8377 = EDGE_CURVE ( 'NONE', #551, #1781, #11343, .T. ) ;
#8378 = FACE_OUTER_BOUND ( 'NONE', #14270, .T. ) ;
#8379 = CIRCLE ( 'NONE', #5947, 9.974999999999999645 ) ;
#8380 = CARTESIAN_POINT ( 'NONE',  ( -7.754796638793765240, -46.50763592918296752, 17.00313569000094560 ) ) ;
#8381 = LINE ( 'NONE', #3876, #9607 ) ;
#8382 = ADVANCED_FACE ( 'NONE', ( #9477 ), #8712, .T. ) ;
#8383 = ORIENTED_EDGE ( 'NONE', *, *, #9529, .T. ) ;
#8384 = CIRCLE ( 'NONE', #8132, 8.000000000000000000 ) ;
#8385 = CARTESIAN_POINT ( 'NONE',  ( -22.80943503306989584, -20.29474937510043731, 57.00231026484397745 ) ) ;
#8386 = AXIS2_PLACEMENT_3D ( 'NONE', #6683, #11367, #890 ) ;
#8387 = DIRECTION ( 'NONE',  ( 8.018662683283438208E-16, -5.975035461963189015E-16, -1.000000000000000000 ) ) ;
#8388 = ORIENTED_EDGE ( 'NONE', *, *, #13296, .T. ) ;
#8389 = PLANE ( 'NONE',  #11953 ) ;
#8390 = FACE_OUTER_BOUND ( 'NONE', #14238, .T. ) ;
#8391 = VERTEX_POINT ( 'NONE', #8087 ) ;
#8392 = CARTESIAN_POINT ( 'NONE',  ( -15.49969986081092088, -13.50737899243822504, 56.85231026484398598 ) ) ;
#8393 = ORIENTED_EDGE ( 'NONE', *, *, #1369, .T. ) ;
#8394 = DIRECTION ( 'NONE',  ( 0.000000000000000000, -1.000000000000000000, -1.224646799147350002E-16 ) ) ;
#8395 = CARTESIAN_POINT ( 'NONE',  ( -10.90377457632059865, -6.867868786151726468, 57.00231026484397745 ) ) ;
#8396 = MECHANICAL_DESIGN_GEOMETRIC_PRESENTATION_REPRESENTATION (  '', ( #842 ), #6919 ) ;
#8397 = CARTESIAN_POINT ( 'NONE',  ( -11.61446667642527331, -19.42012692406430574, 57.00231026484399166 ) ) ;
#8398 = CARTESIAN_POINT ( 'NONE',  ( -15.49969986081099904, 70.81438635534659909, 30.46206422150100934 ) ) ;
#8399 = EDGE_CURVE ( 'NONE', #13135, #8450, #2373, .T. ) ;
#8400 = DIRECTION ( 'NONE',  ( 0.000000000000000000, 0.000000000000000000, 1.000000000000000000 ) ) ;
#8401 = ADVANCED_FACE ( 'NONE', ( #15064 ), #2595, .T. ) ;
#8402 = AXIS2_PLACEMENT_3D ( 'NONE', #1564, #11043, #1491 ) ;
#8403 = CARTESIAN_POINT ( 'NONE',  ( -15.49969986081100259, -19.50737899243800300, 48.00231026484399877 ) ) ;
#8404 = EDGE_CURVE ( 'NONE', #12566, #2877, #11695, .T. ) ;
#8405 = CARTESIAN_POINT ( 'NONE',  ( -8.559186161507744472, -48.52014164539353658, -17.35099849220764412 ) ) ;
#8406 = LINE ( 'NONE', #5122, #2640 ) ;
#8407 = VECTOR ( 'NONE', #8072, 1000.000000000000000 ) ;
#8408 = CARTESIAN_POINT ( 'NONE',  ( -23.49969986081099194, -49.19367049345326137, -0.8113982341407305343 ) ) ;
#8409 = ORIENTED_EDGE ( 'NONE', *, *, #5275, .F. ) ;
#8410 = FACE_OUTER_BOUND ( 'NONE', #7020, .T. ) ;
#8411 = ORIENTED_EDGE ( 'NONE', *, *, #4106, .T. ) ;
#8413 = ORIENTED_EDGE ( 'NONE', *, *, #11703, .T. ) ;
#8412 = CARTESIAN_POINT ( 'NONE',  ( -13.96026682931439034, -23.36287344688023992, 54.00231026484399166 ) ) ;
#8414 = ADVANCED_FACE ( 'NONE', ( #1449 ), #10397, .F. ) ;
#8415 = ORIENTED_EDGE ( 'NONE', *, *, #13571, .T. ) ;
#8416 = FACE_OUTER_BOUND ( 'NONE', #7760, .T. ) ;
#8417 = ORIENTED_EDGE ( 'NONE', *, *, #2725, .T. ) ;
#8418 = CARTESIAN_POINT ( 'NONE',  ( 22.00030013918900096, -27.00737899243800300, 20.96206422150100224 ) ) ;
#8419 = CARTESIAN_POINT ( 'NONE',  ( -10.02446058099324588, -7.572113216692248017, 56.85231026484398598 ) ) ;
#8420 = VECTOR ( 'NONE', #12784, 1000.000000000000000 ) ;
#8421 = EDGE_CURVE ( 'NONE', #1793, #14007, #14340, .T. ) ;
#8422 = CARTESIAN_POINT ( 'NONE',  ( -15.42469993581076970, -26.50737899243800300, 57.00223526491900117 ) ) ;
#8423 = CARTESIAN_POINT ( 'NONE',  ( 0.000000000000000000, 0.000000000000000000, 0.000000000000000000 ) ) ;
#8424 = EDGE_CURVE ( 'NONE', #6799, #3424, #2123, .T. ) ;
#8425 = CARTESIAN_POINT ( 'NONE',  ( 18.44214592757203519, -25.87850161324475451, 8.268049333039575899 ) ) ;
#8426 = CARTESIAN_POINT ( 'NONE',  ( -8.744347237509680681, -17.93190845158491342, 56.85231026484400019 ) ) ;
#8427 = ORIENTED_EDGE ( 'NONE', *, *, #7932, .T. ) ;
#8428 = CARTESIAN_POINT ( 'NONE',  ( 6.023498351796789940, -37.22897031456926698, -11.20623205539177825 ) ) ;
#8429 = ORIENTED_EDGE ( 'NONE', *, *, #2978, .F. ) ;
#8430 = DIRECTION ( 'NONE',  ( 0.4895147004624045839, -0.8719950447285823580, 9.135454576426008610E-16 ) ) ;
#8431 = CARTESIAN_POINT ( 'NONE',  ( -9.328067836852527606, -18.71527762440592468, 56.85231026484400019 ) ) ;
#8432 = ORIENTED_EDGE ( 'NONE', *, *, #8276, .F. ) ;
#8433 = EDGE_LOOP ( 'NONE', ( #2598, #10521, #4483, #2037 ) ) ;
#8434 = CIRCLE ( 'NONE', #1839, 22.99999999999999645 ) ;
#8435 = LINE ( 'NONE', #6124, #3227 ) ;
#8436 = EDGE_LOOP ( 'NONE', ( #12868, #14084, #8120, #14963 ) ) ;
#8437 = CARTESIAN_POINT ( 'NONE',  ( -15.49969986081099904, 10.68321993080349763, 24.21206422150099868 ) ) ;
#8439 = EDGE_CURVE ( 'NONE', #9717, #10845, #6244, .T. ) ;
#8438 = CARTESIAN_POINT ( 'NONE',  ( -8.430459378593662123, -7.816413432484393020, 56.85231026484400019 ) ) ;
#8440 = FACE_OUTER_BOUND ( 'NONE', #2880, .T. ) ;
#8441 = CARTESIAN_POINT ( 'NONE',  ( -15.49969986081092088, -13.50737899243822504, 57.00231026484397745 ) ) ;
#8442 = VECTOR ( 'NONE', #5634, 1000.000000000000000 ) ;
#8443 = PLANE ( 'NONE',  #11584 ) ;
#8445 = LINE ( 'NONE', #9370, #695 ) ;
#8444 = DIRECTION ( 'NONE',  ( 8.018662683283438208E-16, -5.975035461963189015E-16, -1.000000000000000000 ) ) ;
#8446 = VERTEX_POINT ( 'NONE', #10781 ) ;
#8447 = CARTESIAN_POINT ( 'NONE',  ( -15.49969986081099904, 64.39262100756199914, 17.96206422150100579 ) ) ;
#8448 = CARTESIAN_POINT ( 'NONE',  ( -15.73714326519009354, -16.60406334235995018, 57.00231026484397745 ) ) ;
#8449 = ORIENTED_EDGE ( 'NONE', *, *, #13236, .T. ) ;
#8450 = VERTEX_POINT ( 'NONE', #5262 ) ;
#8451 = CARTESIAN_POINT ( 'NONE',  ( 21.89421144759936766, -28.63483922330976483, 21.39079340381945471 ) ) ;
#8452 = LINE ( 'NONE', #5997, #14711 ) ;
#8453 = ORIENTED_EDGE ( 'NONE', *, *, #7276, .T. ) ;
#8454 = CARTESIAN_POINT ( 'NONE',  ( -8.313732008561206754, -40.95305761153253599, -17.30330790116151007 ) ) ;
#8455 = EDGE_CURVE ( 'NONE', #3528, #7352, #13314, .T. ) ;
#8456 = EDGE_CURVE ( 'NONE', #964, #13913, #2671, .T. ) ;
#8457 = AXIS2_PLACEMENT_3D ( 'NONE', #1992, #6714, #10248 ) ;
#8458 = CARTESIAN_POINT ( 'NONE',  ( -15.49969986081092088, -13.50737899243822504, 56.85231026484398598 ) ) ;
#8459 = DIRECTION ( 'NONE',  ( 0.000000000000000000, -1.000000000000000000, -1.224646799147350002E-16 ) ) ;
#8460 = CARTESIAN_POINT ( 'NONE',  ( -7.498776711167360887, -44.75663421272680864, 17.70716976648120422 ) ) ;
#8461 = DIRECTION ( 'NONE',  ( 1.000000000000000000, 3.700743415417188632E-16, 0.000000000000000000 ) ) ;
#8462 = EDGE_LOOP ( 'NONE', ( #1492, #7248, #5156, #4224 ) ) ;
#8463 = CARTESIAN_POINT ( 'NONE',  ( -1.821162622431179878, -46.50737899243799234, -5.497689735156000346 ) ) ;
#8464 = VECTOR ( 'NONE', #8017, 1000.000000000000000 ) ;
#8465 = CARTESIAN_POINT ( 'NONE',  ( -25.46211945451987191, -14.00819915864900977, 54.00231026484397745 ) ) ;
#8466 = VERTEX_POINT ( 'NONE', #524 ) ;
#8467 = FACE_OUTER_BOUND ( 'NONE', #9519, .T. ) ;
#8468 = ORIENTED_EDGE ( 'NONE', *, *, #14204, .F. ) ;
#8469 = DIRECTION ( 'NONE',  ( -1.000000000000000000, 0.000000000000000000, 0.000000000000000000 ) ) ;
#8470 = VERTEX_POINT ( 'NONE', #5184 ) ;
#8471 = AXIS2_PLACEMENT_3D ( 'NONE', #1326, #7272, #342 ) ;
#8472 = DIRECTION ( 'NONE',  ( 8.018662683283438208E-16, -5.975035461963189015E-16, -1.000000000000000000 ) ) ;
#8473 = ADVANCED_FACE ( 'NONE', ( #2821 ), #13139, .T. ) ;
#8474 = CARTESIAN_POINT ( 'NONE',  ( -10.07958688850791162, -7.521259601090221736, 57.00231026484397745 ) ) ;
#8475 = DIRECTION ( 'NONE',  ( 1.000000000000000000, 1.000000000000000078E-15, 0.000000000000000000 ) ) ;
#8476 = VECTOR ( 'NONE', #1374, 1000.000000000000000 ) ;
#8477 = DIRECTION ( 'NONE',  ( -1.000000000000000000, 0.000000000000000000, 0.000000000000000000 ) ) ;
#8478 = AXIS2_PLACEMENT_3D ( 'NONE', #220, #296, #14214 ) ;
#8479 = CARTESIAN_POINT ( 'NONE',  ( -15.49969986081091378, -13.50737899243822859, 51.00231026484399166 ) ) ;
#8480 = ORIENTED_EDGE ( 'NONE', *, *, #2519, .T. ) ;
#8481 = CARTESIAN_POINT ( 'NONE',  ( -8.011459754790374532, -47.33491808379935861, -17.24257761966661917 ) ) ;
#8482 = CARTESIAN_POINT ( 'NONE',  ( -14.61203582817000068, -106.2504778273845147, -6.614114137688406281 ) ) ;
#8483 = CARTESIAN_POINT ( 'NONE',  ( -15.31527533914055539, -21.58027268651140673, 57.00231026484399166 ) ) ;
#8484 = ORIENTED_EDGE ( 'NONE', *, *, #914, .F. ) ;
#8485 = CARTESIAN_POINT ( 'NONE',  ( -21.21771647519868154, -9.340181373223902739, 57.00231026484397745 ) ) ;
#8486 = EDGE_LOOP ( 'NONE', ( #3298, #6691, #3285, #10409, #5655 ) ) ;
#8488 = ORIENTED_EDGE ( 'NONE', *, *, #9684, .T. ) ;
#8487 = CARTESIAN_POINT ( 'NONE',  ( -17.81448839017817320, -11.78253482624721116, 56.89875687425070794 ) ) ;
#8489 = VERTEX_POINT ( 'NONE', #14301 ) ;
#8490 = EDGE_CURVE ( 'NONE', #10768, #11542, #12636, .T. ) ;
#8491 = CARTESIAN_POINT ( 'NONE',  ( -18.23096777355884157, -13.18694867428211914, 56.75231026484397745 ) ) ;
#8492 = LINE ( 'NONE', #6481, #9992 ) ;
#8493 = EDGE_CURVE ( 'NONE', #5861, #9932, #4044, .T. ) ;
#8494 = CARTESIAN_POINT ( 'NONE',  ( -21.45979773411919567, -21.50599501901345789, 48.00231026484398456 ) ) ;
#8495 = B_SPLINE_CURVE_WITH_KNOTS ( 'NONE', 3,
 ( #9692, #10844, #2809, #10916 ),
 .UNSPECIFIED., .F., .F.,
 ( 4, 4 ),
 ( 0.000000000000000000, 1.000000000000000000 ),
 .UNSPECIFIED. ) ;
#8496 = DIRECTION ( 'NONE',  ( 8.018662683283438208E-16, -5.975035461963189015E-16, -1.000000000000000000 ) ) ;
#8497 = DIRECTION ( 'NONE',  ( 5.366764484277593297E-17, -0.4874022346767251657, -0.8731775659235267995 ) ) ;
#8498 = CIRCLE ( 'NONE', #11925, 8.000000000000000000 ) ;
#8499 = DIRECTION ( 'NONE',  ( -0.3956847857120157075, 0.9183863840214729901, -8.660254037844387408E-16 ) ) ;
#8500 = VECTOR ( 'NONE', #8981, 1000.000000000000000 ) ;
#8501 = VECTOR ( 'NONE', #14730, 1000.000000000000000 ) ;
#8502 = CARTESIAN_POINT ( 'NONE',  ( -15.49969986081099904, 3.992621007561997892, 24.21206422150099868 ) ) ;
#8503 = CARTESIAN_POINT ( 'NONE',  ( -15.49969986081099904, 10.68321993080349763, 24.21206422150099868 ) ) ;
#8504 = ORIENTED_EDGE ( 'NONE', *, *, #7928, .F. ) ;
#8505 = DIRECTION ( 'NONE',  ( 0.000000000000000000, 0.000000000000000000, 1.000000000000000000 ) ) ;
#8506 = ORIENTED_EDGE ( 'NONE', *, *, #1396, .F. ) ;
#8507 = ORIENTED_EDGE ( 'NONE', *, *, #562, .T. ) ;
#8508 = EDGE_CURVE ( 'NONE', #2702, #13947, #1836, .T. ) ;
#8509 = DIRECTION ( 'NONE',  ( -8.018662683283438208E-16, 5.975035461963189015E-16, 1.000000000000000000 ) ) ;
#8510 = ADVANCED_FACE ( 'NONE', ( #671 ), #4268, .F. ) ;
#8511 = ORIENTED_EDGE ( 'NONE', *, *, #3027, .F. ) ;
#8512 = EDGE_LOOP ( 'NONE', ( #1274, #11958, #8969, #2489 ) ) ;
#8513 = PLANE ( 'NONE',  #14725 ) ;
#8514 = DIRECTION ( 'NONE',  ( 0.000000000000000000, 1.224646799147350002E-16, -1.000000000000000000 ) ) ;
#8515 = PLANE ( 'NONE',  #2891 ) ;
#8516 =( GEOMETRIC_REPRESENTATION_CONTEXT ( 3 ) GLOBAL_UNCERTAINTY_ASSIGNED_CONTEXT ( ( #5735 ) ) GLOBAL_UNIT_ASSIGNED_CONTEXT ( ( #10106, #2089, #10416 ) ) REPRESENTATION_CONTEXT ( 'NONE', 'WORKASPACE' ) );
#8517 = DIRECTION ( 'NONE',  ( 0.000000000000000000, 0.000000000000000000, 1.000000000000000000 ) ) ;
#8518 = CARTESIAN_POINT ( 'NONE',  ( -9.565488148413145097, -20.37370125056455095, 57.00231026484399166 ) ) ;
#8519 = CLOSED_SHELL ( 'NONE', ( #1680, #435, #13568, #2893, #809, #9422, #10230, #4043, #10702, #759, #13900, #13965, #13588, #1016, #12227, #8112, #10926, #4512, #458, #9456, #12296, #9148, #1141, #5045, #9510, #2012, #11493, #2252, #4645, #7267, #314, #6865, #7531, #8332, #6802, #2, #7716, #5974, #11566, #14540, #13861, #4514, #11631, #7472, #13473, #12843, #8627, #10651, #11252, #7886, #2881, #1779, #5163, #8294, #13581, #2838, #5422, #7817 ) ) ;
#8520 = EDGE_LOOP ( 'NONE', ( #12997, #8993, #12499, #6223, #4828, #5161, #243, #12946, #14051, #2224, #14190, #3304, #2720, #2385, #244, #5494, #13701, #11982, #9791, #8157, #5411, #3448, #2713, #5963, #8522, #8670, #14046 ) ) ;
#8521 = FACE_OUTER_BOUND ( 'NONE', #6026, .T. ) ;
#8522 = ORIENTED_EDGE ( 'NONE', *, *, #9723, .T. ) ;
#8523 = EDGE_LOOP ( 'NONE', ( #7629, #10215, #12597, #13582, #10349, #9805 ) ) ;
#8524 = CARTESIAN_POINT ( 'NONE',  ( -20.54757852167729837, -19.81012014412530320, 56.85231026484398598 ) ) ;
#8525 = B_SPLINE_CURVE_WITH_KNOTS ( 'NONE', 3,
 ( #13544, #3133, #12549, #7707, #12392, #5569, #4281, #10011, #10156, #13764, #992, #6560, #3290, #9013, #6709, #12624, #11244, #2139, #2066, #765, #7784, #6785, #10082, #5421, #7853, #8938 ),
 .UNSPECIFIED., .F., .F.,
 ( 4, 2, 2, 2, 2, 2, 2, 2, 2, 2, 2, 2, 4 ),
 ( 0.03783275914711289878, 0.03940993297411544971, 0.04019851988761673905, 0.04098710680111802840, 0.04177569371461931774, 0.04256428062812060015, 0.04414145445512319965, 0.04493004136862448900, 0.04571862828212578528, 0.04729580210912836397, 0.04808438902262963943, 0.04887297593613092878, 0.05045014976313349359 ),
 .UNSPECIFIED. ) ;
#8526 = CARTESIAN_POINT ( 'NONE',  ( -22.68842631263146004, -48.05638050496262537, 56.30739098709261725 ) ) ;
#8527 = EDGE_CURVE ( 'NONE', #7429, #8707, #6697, .T. ) ;
#8528 = ORIENTED_EDGE ( 'NONE', *, *, #14106, .F. ) ;
#8529 = VECTOR ( 'NONE', #6928, 1000.000000000000000 ) ;
#8530 = CARTESIAN_POINT ( 'NONE',  ( -15.49969986081099727, 22.99262100756199700, 39.83706422150100224 ) ) ;
#8531 = AXIS2_PLACEMENT_3D ( 'NONE', #7422, #8497, #1897 ) ;
#8532 = ADVANCED_FACE ( 'NONE', ( #12459 ), #4421, .T. ) ;
#8533 = FACE_OUTER_BOUND ( 'NONE', #9236, .T. ) ;
#8534 = CARTESIAN_POINT ( 'NONE',  ( 3.243537350957551357, 11.48902252484887399, 32.26206422150129072 ) ) ;
#8535 = AXIS2_PLACEMENT_3D ( 'NONE', #14857, #13710, #3231 ) ;
#8536 = AXIS2_PLACEMENT_3D ( 'NONE', #8923, #5405, #11299 ) ;
#8537 = EDGE_CURVE ( 'NONE', #9493, #5899, #6981, .T. ) ;
#8538 = CARTESIAN_POINT ( 'NONE',  ( -7.532288152704643025, -45.22345379519396857, 17.35487173259670612 ) ) ;
#8539 = CARTESIAN_POINT ( 'NONE',  ( -3.508527451664999575, -46.50737899243799234, -3.997689735156000790 ) ) ;
#8540 = ORIENTED_EDGE ( 'NONE', *, *, #7088, .T. ) ;
#8541 = DIRECTION ( 'NONE',  ( -1.000000000000000000, 0.000000000000000000, -1.011922027653137143E-15 ) ) ;
#8542 = FACE_OUTER_BOUND ( 'NONE', #14934, .T. ) ;
#8543 = EDGE_LOOP ( 'NONE', ( #2019, #8895 ) ) ;
#8544 = DIRECTION ( 'NONE',  ( 0.000000000000000000, 0.000000000000000000, -1.000000000000000000 ) ) ;
#8545 = VERTEX_POINT ( 'NONE', #14972 ) ;
#8546 = CARTESIAN_POINT ( 'NONE',  ( -8.992083836518990125, -50.38952316532486009, 13.62016609195713812 ) ) ;
#8547 = EDGE_LOOP ( 'NONE', ( #6277, #10506, #3801, #4412 ) ) ;
#8548 = DIRECTION ( 'NONE',  ( 0.5975035461963189576, 0.8018662683283437342, 0.000000000000000000 ) ) ;
#8549 = CARTESIAN_POINT ( 'NONE',  ( -15.49969986081100437, -101.1160386300729357, -6.570400712645788843 ) ) ;
#8550 = DIRECTION ( 'NONE',  ( -1.000000000000000000, 0.000000000000000000, 0.000000000000000000 ) ) ;
#8551 = CARTESIAN_POINT ( 'NONE',  ( -7.719139325354706926, -48.17958124988508928, 17.64249027060945352 ) ) ;
#8552 = CONICAL_SURFACE ( 'NONE', #14913, 1.300000000000000488, 0.1221730476396025861 ) ;
#8553 = EDGE_CURVE ( 'NONE', #6540, #11437, #7694, .T. ) ;
#8554 = CARTESIAN_POINT ( 'NONE',  ( 16.90967644101677081, -30.26063172738379237, 5.345825581268424997 ) ) ;
#8555 = LINE ( 'NONE', #10498, #1333 ) ;
#8556 = VERTEX_POINT ( 'NONE', #5486 ) ;
#8557 = CARTESIAN_POINT ( 'NONE',  ( -7.499699860810999041, -44.50737899243799944, -17.13441993860073964 ) ) ;
#8558 = DIRECTION ( 'NONE',  ( -0.5975035461963187355, -0.8018662683283439563, 0.000000000000000000 ) ) ;
#8559 = ORIENTED_EDGE ( 'NONE', *, *, #4190, .F. ) ;
#8560 = CARTESIAN_POINT ( 'NONE',  ( -15.49969986081092088, -13.50737899243822504, 56.85231026484398598 ) ) ;
#8561 = VERTEX_POINT ( 'NONE', #4496 ) ;
#8563 = ORIENTED_EDGE ( 'NONE', *, *, #1394, .T. ) ;
#8562 = CARTESIAN_POINT ( 'NONE',  ( -35.09539592173130274, -38.34531428876476866, -12.47047561222863266 ) ) ;
#8564 = VERTEX_POINT ( 'NONE', #12378 ) ;
#8565 = DIRECTION ( 'NONE',  ( -8.018662683283438208E-16, 5.975035461963189015E-16, 1.000000000000000000 ) ) ;
#8566 = CARTESIAN_POINT ( 'NONE',  ( -15.10625462230756177, -3.540141368888813922, 57.00231026484397745 ) ) ;
#8567 = DIRECTION ( 'NONE',  ( 8.018662683283438208E-16, -5.975035461963189015E-16, -1.000000000000000000 ) ) ;
#8568 = CARTESIAN_POINT ( 'NONE',  ( -11.65397503470588703, -4.262226922354281911, 61.51805161050018711 ) ) ;
#8569 = PRODUCT_CONTEXT ( 'NONE', #4007, 'mechanical' ) ;
#8570 = DIRECTION ( 'NONE',  ( 0.000000000000000000, -1.000000000000000000, -1.224646799147350002E-16 ) ) ;
#8571 = ADVANCED_FACE ( 'NONE', ( #4348 ), #1898, .T. ) ;
#8572 = LINE ( 'NONE', #2768, #5787 ) ;
#8573 = DIRECTION ( 'NONE',  ( 0.000000000000000000, -1.000000000000000000, -1.224646799147350002E-16 ) ) ;
#8574 = ADVANCED_FACE ( 'NONE', ( #6547 ), #9074, .F. ) ;
#8575 = LINE ( 'NONE', #5286, #7108 ) ;
#8576 = ORIENTED_EDGE ( 'NONE', *, *, #10942, .T. ) ;
#8577 = CARTESIAN_POINT ( 'NONE',  ( -22.13265177292497299, -18.11337496850924822, 57.00231026484397745 ) ) ;
#8578 = VERTEX_POINT ( 'NONE', #5406 ) ;
#8579 = ORIENTED_EDGE ( 'NONE', *, *, #7276, .F. ) ;
#8580 = LINE ( 'NONE', #2777, #307 ) ;
#8581 = ORIENTED_EDGE ( 'NONE', *, *, #10140, .F. ) ;
#8582 = CONICAL_SURFACE ( 'NONE', #5888, 19.00000000000000000, 1.047197551196598297 ) ;
#8583 = DIRECTION ( 'NONE',  ( 0.5975035461963189576, 0.8018662683283437342, 0.000000000000000000 ) ) ;
#8584 = DIRECTION ( 'NONE',  ( -8.018662683283439195E-16, 5.975035461963190001E-16, 1.000000000000000000 ) ) ;
#8585 = DIRECTION ( 'NONE',  ( 0.6780482080269577549, 0.7350174335289139105, 1.045284632676540317E-16 ) ) ;
#8586 = EDGE_CURVE ( 'NONE', #5325, #12427, #13604, .T. ) ;
#8587 = AXIS2_PLACEMENT_3D ( 'NONE', #7432, #2701, #7654 ) ;
#8588 = EDGE_CURVE ( 'NONE', #13854, #8833, #10143, .T. ) ;
#8589 = CIRCLE ( 'NONE', #3214, 5.000000000000000000 ) ;
#8590 = CARTESIAN_POINT ( 'NONE',  ( -24.08903783298838519, -16.43731469134198520, 56.85231026484398598 ) ) ;
#8591 = PRODUCT_DEFINITION_SHAPE ( 'NONE', 'NONE',  #15129 ) ;
#8593 = DIRECTION ( 'NONE',  ( -8.018662683283438208E-16, 5.975035461963189015E-16, 1.000000000000000000 ) ) ;
#8592 = CARTESIAN_POINT ( 'NONE',  ( -7.516520390631882265, -48.95538363176678587, -6.022680771983879744 ) ) ;
#8594 = EDGE_CURVE ( 'NONE', #9544, #12009, #3342, .T. ) ;
#8595 = VERTEX_POINT ( 'NONE', #12609 ) ;
#8596 = CARTESIAN_POINT ( 'NONE',  ( -9.291286065451622278, -6.887949398765353060, 56.85231026484398598 ) ) ;
#8597 = ORIENTED_EDGE ( 'NONE', *, *, #11908, .F. ) ;
#8598 = CARTESIAN_POINT ( 'NONE',  ( -15.49969986081099904, 71.39262100756199914, 31.04029887371640939 ) ) ;
#8599 = EDGE_LOOP ( 'NONE', ( #718, #11979 ) ) ;
#8600 = EDGE_LOOP ( 'NONE', ( #3713, #1700 ) ) ;
#8601 = DIRECTION ( 'NONE',  ( 8.018662683283438208E-16, -5.975035461963189015E-16, -1.000000000000000000 ) ) ;
#8602 = DIRECTION ( 'NONE',  ( 0.8543800322332385511, 0.5196486895212286683, 3.746065934159130275E-16 ) ) ;
#8603 = ORIENTED_EDGE ( 'NONE', *, *, #6988, .T. ) ;
#8604 = EDGE_CURVE ( 'NONE', #4315, #4372, #1823, .T. ) ;
#8605 = AXIS2_PLACEMENT_3D ( 'NONE', #13451, #12449, #2956 ) ;
#8606 = VECTOR ( 'NONE', #471, 1000.000000000000114 ) ;
#8607 = AXIS2_PLACEMENT_3D ( 'NONE', #13454, #13233, #1736 ) ;
#8608 = AXIS2_PLACEMENT_3D ( 'NONE', #9401, #9166, #7939 ) ;
#8609 = CARTESIAN_POINT ( 'NONE',  ( -20.87112600995946110, -106.2635794615412834, -5.497689735156005675 ) ) ;
#8610 = CARTESIAN_POINT ( 'NONE',  ( -11.02548131428532940, -22.45062562374627291, 56.73443632552402249 ) ) ;
#8611 = EDGE_CURVE ( 'NONE', #10009, #7867, #9703, .T. ) ;
#8612 = CARTESIAN_POINT ( 'NONE',  ( -7.517689378148951107, -45.05639236071581166, 17.46402815569863876 ) ) ;
#8613 = LINE ( 'NONE', #7458, #14265 ) ;
#8614 = ORIENTED_EDGE ( 'NONE', *, *, #6443, .T. ) ;
#8615 = LINE ( 'NONE', #9913, #10682 ) ;
#8616 = CIRCLE ( 'NONE', #11966, 1.744527686444488968 ) ;
#8617 =( BOUNDED_CURVE ( )  B_SPLINE_CURVE ( 3, ( #213, #1507, #1434, #6006 ),
 .UNSPECIFIED., .F., .T. ) 
 B_SPLINE_CURVE_WITH_KNOTS ( ( 4, 4 ),
 ( -8.881784197001252323E-16, 1.570796326794893893 ),
 .UNSPECIFIED. ) 
 CURVE ( )  GEOMETRIC_REPRESENTATION_ITEM ( )  RATIONAL_B_SPLINE_CURVE ( ( 1.000000000000000000, 0.8047378541243654926, 0.8047378541243654926, 1.000000000000000000 ) ) 
 REPRESENTATION_ITEM ( '' )  );
#8618 = CARTESIAN_POINT ( 'NONE',  ( -15.47224238247604511, -13.54916519690201149, 56.85231026484398598 ) ) ;
#8619 = ORIENTED_EDGE ( 'NONE', *, *, #9684, .F. ) ;
#8620 = CIRCLE ( 'NONE', #2025, 3.000000000000000000 ) ;
#8621 = CARTESIAN_POINT ( 'NONE',  ( 21.86106836617108939, -26.57972102403619630, 20.98332789618103078 ) ) ;
#8622 = SURFACE_STYLE_USAGE ( .BOTH. , #447 ) ;
#8623 = VERTEX_POINT ( 'NONE', #2599 ) ;
#8624 = CARTESIAN_POINT ( 'NONE',  ( -17.87376992080280758, -22.26666214519964271, 56.85231026484400019 ) ) ;
#8625 = EDGE_LOOP ( 'NONE', ( #14062, #13649, #13595, #9808 ) ) ;
#8626 = CARTESIAN_POINT ( 'NONE',  ( -15.49969986081092088, -13.50737899243822504, 57.00231026484397745 ) ) ;
#8627 = ADVANCED_FACE ( 'NONE', ( #11854 ), #14154, .F. ) ;
#8628 = CARTESIAN_POINT ( 'NONE',  ( -20.87112600995945755, -110.0073789924380065, -5.497689735156006563 ) ) ;
#8629 = AXIS2_PLACEMENT_3D ( 'NONE', #7630, #5269, #12313 ) ;
#8630 = CARTESIAN_POINT ( 'NONE',  ( -7.795459123704175042, -47.76474896896232281, 17.34149980383660861 ) ) ;
#8631 = VECTOR ( 'NONE', #12746, 1000.000000000000114 ) ;
#8632 = CARTESIAN_POINT ( 'NONE',  ( 18.47602945437533251, -27.91681196510473484, 8.340622674467514486 ) ) ;
#8633 = DIRECTION ( 'NONE',  ( -8.018662683283438208E-16, 5.975035461963189015E-16, 1.000000000000000000 ) ) ;
#8634 = ORIENTED_EDGE ( 'NONE', *, *, #5168, .F. ) ;
#8635 = CARTESIAN_POINT ( 'NONE',  ( 13.85920135429429934, -27.00737899243800300, 24.21206422150099868 ) ) ;
#8636 = CARTESIAN_POINT ( 'NONE',  ( -16.49725497239786520, -3.582384846377123733, 57.00231026484397745 ) ) ;
#8637 = ORIENTED_EDGE ( 'NONE', *, *, #6346, .T. ) ;
#8638 = VERTEX_POINT ( 'NONE', #8325 ) ;
#8640 = VERTEX_POINT ( 'NONE', #10784 ) ;
#8639 = CARTESIAN_POINT ( 'NONE',  ( -12.81093390292747536, -9.898980784960686563, 46.00231026484398456 ) ) ;
#8641 = ORIENTED_EDGE ( 'NONE', *, *, #10445, .F. ) ;
#8642 = VECTOR ( 'NONE', #10371, 1000.000000000000114 ) ;
#8643 = LINE ( 'NONE', #13251, #1611 ) ;
#8644 = ORIENTED_EDGE ( 'NONE', *, *, #6147, .T. ) ;
#8645 = EDGE_CURVE ( 'NONE', #5527, #9881, #6099, .T. ) ;
#8646 = DIRECTION ( 'NONE',  ( -8.018662683283438208E-16, 5.975035461963189015E-16, 1.000000000000000000 ) ) ;
#8647 = CARTESIAN_POINT ( 'NONE',  ( -10.20730426669924995, -5.016324734929597184, 61.33773678374165428 ) ) ;
#8648 = FACE_OUTER_BOUND ( 'NONE', #7041, .T. ) ;
#8649 = AXIS2_PLACEMENT_3D ( 'NONE', #1670, #2894, #9784 ) ;
#8650 = CARTESIAN_POINT ( 'NONE',  ( -14.10579935493720782, -22.47500361547664127, 56.85231026484400019 ) ) ;
#8651 = ORIENTED_EDGE ( 'NONE', *, *, #12141, .T. ) ;
#8652 = DIRECTION ( 'NONE',  ( -0.9183863840214729901, -0.3956847857120157075, -4.999999999999999402E-16 ) ) ;
#8653 = ORIENTED_EDGE ( 'NONE', *, *, #10478, .F. ) ;
#8654 = DIRECTION ( 'NONE',  ( -1.000000000000000000, -1.000000000000000078E-15, -0.000000000000000000 ) ) ;
#8655 = AXIS2_PLACEMENT_3D ( 'NONE', #3631, #8285, #4863 ) ;
#8656 = ORIENTED_EDGE ( 'NONE', *, *, #2164, .T. ) ;
#8657 = ORIENTED_EDGE ( 'NONE', *, *, #11956, .T. ) ;
#8658 = CARTESIAN_POINT ( 'NONE',  ( -3.508527451664998686, -47.80641709811465745, -6.247689735156000346 ) ) ;
#8659 = EDGE_LOOP ( 'NONE', ( #13062, #10594 ) ) ;
#8660 = CARTESIAN_POINT ( 'NONE',  ( -11.02821192705052233, -12.92121384215898416, -13.02043737883916208 ) ) ;
#8661 = AXIS2_PLACEMENT_3D ( 'NONE', #8824, #12433, #730 ) ;
#8662 = ADVANCED_FACE ( 'NONE', ( #8250 ), #9786, .T. ) ;
#8663 = CYLINDRICAL_SURFACE ( 'NONE', #7804, 1.750000000000000666 ) ;
#8664 = CARTESIAN_POINT ( 'NONE',  ( -7.654212976755197850, -10.04550297615607768, 56.85231026484400019 ) ) ;
#8665 = AXIS2_PLACEMENT_3D ( 'NONE', #11867, #7030, #3608 ) ;
#8666 = DIRECTION ( 'NONE',  ( 1.224646799147350002E-16, 1.224646799147350002E-16, -1.000000000000000000 ) ) ;
#8667 = ORIENTED_EDGE ( 'NONE', *, *, #5143, .F. ) ;
#8668 = LINE ( 'NONE', #1712, #453 ) ;
#8669 = PLANE ( 'NONE',  #6001 ) ;
#8670 = ORIENTED_EDGE ( 'NONE', *, *, #7943, .T. ) ;
#8671 = EDGE_LOOP ( 'NONE', ( #891, #10424, #14831, #14241 ) ) ;
#8672 = DIRECTION ( 'NONE',  ( -0.8885476655824650072, -0.4587843131450243805, -4.383711467890778149E-16 ) ) ;
#8673 = ORIENTED_EDGE ( 'NONE', *, *, #5985, .T. ) ;
#8674 = DIRECTION ( 'NONE',  ( 8.018662683283438208E-16, -5.975035461963189015E-16, -1.000000000000000000 ) ) ;
#8675 = EDGE_CURVE ( 'NONE', #6428, #8353, #7407, .T. ) ;
#8676 = EDGE_CURVE ( 'NONE', #14647, #7451, #7730, .T. ) ;
#8677 = CARTESIAN_POINT ( 'NONE',  ( -22.70913108387521007, -17.14542124616560770, 57.00231026484397745 ) ) ;
#8678 = LINE ( 'NONE', #652, #3668 ) ;
#8679 = CARTESIAN_POINT ( 'NONE',  ( -8.703838785437527648, -17.86878899887247130, 57.00231026484399166 ) ) ;
#8680 = EDGE_CURVE ( 'NONE', #2996, #2455, #7092, .T. ) ;
#8681 = CARTESIAN_POINT ( 'NONE',  ( -22.94870171817393256, -18.69135635822624053, 56.85231026484398598 ) ) ;
#8682 = CARTESIAN_POINT ( 'NONE',  ( -12.84854673063649777, -12.36513540471286277, 56.89875687425070794 ) ) ;
#8683 = ORIENTED_EDGE ( 'NONE', *, *, #4586, .T. ) ;
#8684 = CARTESIAN_POINT ( 'NONE',  ( -8.561607448813433052, -9.375294326971793879, 56.85231026484400019 ) ) ;
#8685 = LINE ( 'NONE', #2879, #4488 ) ;
#8686 = ORIENTED_EDGE ( 'NONE', *, *, #4404, .F. ) ;
#8687 = AXIS2_PLACEMENT_3D ( 'NONE', #359, #13577, #4164 ) ;
#8688 = APPLICATION_CONTEXT ( 'automotive_design' ) ;
#8689 = CARTESIAN_POINT ( 'NONE',  ( 21.85920135429435973, -26.79253637162340596, 27.46206422150100224 ) ) ;
#8690 = VERTEX_POINT ( 'NONE', #4976 ) ;
#8691 = EDGE_CURVE ( 'NONE', #7312, #4275, #4903, .T. ) ;
#8692 = AXIS2_PLACEMENT_3D ( 'NONE', #4726, #9388, #15121 ) ;
#8693 = CARTESIAN_POINT ( 'NONE',  ( -15.49969986081092621, -96.50737899243799234, -9.210188241073819171 ) ) ;
#8694 = EDGE_LOOP ( 'NONE', ( #12694, #4389, #3318, #13687 ) ) ;
#8695 = CARTESIAN_POINT ( 'NONE',  ( -8.971570239337626873, -21.04953708182106098, 56.85231026484400019 ) ) ;
#8696 = EDGE_CURVE ( 'NONE', #9374, #7373, #162, .T. ) ;
#8697 = EDGE_CURVE ( 'NONE', #9604, #14718, #10228, .T. ) ;
#8698 = LINE ( 'NONE', #5261, #12457 ) ;
#8699 = CARTESIAN_POINT ( 'NONE',  ( -7.664252951136433012, -48.41696643141915501, 17.88875613834384737 ) ) ;
#8700 =( BOUNDED_CURVE ( )  B_SPLINE_CURVE ( 3, ( #5178, #12223, #6239, #5331 ),
 .UNSPECIFIED., .F., .T. ) 
 B_SPLINE_CURVE_WITH_KNOTS ( ( 4, 4 ),
 ( 1.070141614390309304, 1.245066839500267530 ),
 .UNSPECIFIED. ) 
 CURVE ( )  GEOMETRIC_REPRESENTATION_ITEM ( )  RATIONAL_B_SPLINE_CURVE ( ( 1.000000000000000000, 0.9974517222217440526, 0.9974517222217440526, 1.000000000000000000 ) ) 
 REPRESENTATION_ITEM ( '' )  );
#8701 = DIRECTION ( 'NONE',  ( 0.5975035461963189576, 0.8018662683283437342, 0.000000000000000000 ) ) ;
#8702 = DIRECTION ( 'NONE',  ( 0.000000000000000000, 0.000000000000000000, -1.000000000000000000 ) ) ;
#8703 = ORIENTED_EDGE ( 'NONE', *, *, #8998, .T. ) ;
#8704 = DIRECTION ( 'NONE',  ( -8.018662683283438208E-16, 5.975035461963189015E-16, 1.000000000000000000 ) ) ;
#8705 = DIRECTION ( 'NONE',  ( -8.018662683283438208E-16, 5.975035461963189015E-16, 1.000000000000000000 ) ) ;
#8706 = VERTEX_POINT ( 'NONE', #2752 ) ;
#8707 = VERTEX_POINT ( 'NONE', #12088 ) ;
#8709 = VERTEX_POINT ( 'NONE', #5412 ) ;
#8708 = CARTESIAN_POINT ( 'NONE',  ( -33.91855968657274190, -40.00214821740372884, -13.16261487092677207 ) ) ;
#8710 = ORIENTED_EDGE ( 'NONE', *, *, #1207, .T. ) ;
#8711 = CARTESIAN_POINT ( 'NONE',  ( -16.90917998795211119, -101.9740710344159140, -6.700100522990623197 ) ) ;
#8712 = CONICAL_SURFACE ( 'NONE', #4562, 4.499999999999999112, 0.7853981633974476129 ) ;
#8713 = CARTESIAN_POINT ( 'NONE',  ( -25.29546517631143132, -15.38982603914036140, 56.85231026484398598 ) ) ;
#8714 = EDGE_CURVE ( 'NONE', #1944, #1815, #4423, .T. ) ;
#8715 = DIRECTION ( 'NONE',  ( 0.000000000000000000, -1.000000000000000000, -1.224646799147350002E-16 ) ) ;
#8716 = CYLINDRICAL_SURFACE ( 'NONE', #1338, 0.4500000000000011768 ) ;
#8717 = AXIS2_PLACEMENT_3D ( 'NONE', #14643, #9827, #12199 ) ;
#8718 = PRODUCT_DEFINITION_SHAPE ( 'NONE', 'NONE',  #15130 ) ;
#8719 = DIRECTION ( 'NONE',  ( 0.5975035461963189576, 0.8018662683283437342, 0.000000000000000000 ) ) ;
#8720 = CARTESIAN_POINT ( 'NONE',  ( -15.49969986081099549, 4.873818854045002702, 1.212064221501000461 ) ) ;
#8721 = VECTOR ( 'NONE', #7844, 1000.000000000000114 ) ;
#8722 = EDGE_CURVE ( 'NONE', #1750, #13341, #12651, .T. ) ;
#8723 = CARTESIAN_POINT ( 'NONE',  ( -21.17290370923395670, -9.280041403099277275, 56.85231026484398598 ) ) ;
#8724 = CARTESIAN_POINT ( 'NONE',  ( -15.49969986081099904, -57.00737899243801365, 57.00231026484399166 ) ) ;
#8725 = VERTEX_POINT ( 'NONE', #9927 ) ;
#8726 = DIRECTION ( 'NONE',  ( 0.000000000000000000, 1.000000000000000000, 1.224646799147350002E-16 ) ) ;
#8728 = ORIENTED_EDGE ( 'NONE', *, *, #3027, .T. ) ;
#8727 = CARTESIAN_POINT ( 'NONE',  ( -15.49969986081092088, -13.50737899243822504, 56.85231026484398598 ) ) ;
#8729 = EDGE_LOOP ( 'NONE', ( #11742, #4835, #6572, #13392 ) ) ;
#8730 = DIRECTION ( 'NONE',  ( 0.000000000000000000, -1.000000000000000000, -1.224646799147350002E-16 ) ) ;
#8731 = VERTEX_POINT ( 'NONE', #14755 ) ;
#8732 = PLANE ( 'NONE',  #4881 ) ;
#8733 = AXIS2_PLACEMENT_3D ( 'NONE', #14565, #13429, #7596 ) ;
#8734 = CARTESIAN_POINT ( 'NONE',  ( -7.145558396657055944, -18.95797028117975458, 54.00231026484400587 ) ) ;
#8735 = VECTOR ( 'NONE', #6227, 1000.000000000000227 ) ;
#8736 = DIRECTION ( 'NONE',  ( 0.5975035461963172922, 0.8018662683283449555, 0.000000000000000000 ) ) ;
#8737 = EDGE_CURVE ( 'NONE', #7024, #13353, #5491, .T. ) ;
#8739 = DIRECTION ( 'NONE',  ( 1.000000000000000275E-15, -0.9823027872370663216, 0.1872998510044540654 ) ) ;
#8738 = PLANE ( 'NONE',  #2507 ) ;
#8740 = ORIENTED_EDGE ( 'NONE', *, *, #13016, .F. ) ;
#8741 = CARTESIAN_POINT ( 'NONE',  ( -18.09969986081099336, -109.6731500378498794, -10.30222923886191388 ) ) ;
#8742 = DIRECTION ( 'NONE',  ( 0.5975035461963187355, 0.8018662683283439563, 0.000000000000000000 ) ) ;
#8743 = ORIENTED_EDGE ( 'NONE', *, *, #193, .F. ) ;
#8744 = ORIENTED_EDGE ( 'NONE', *, *, #6824, .T. ) ;
#8745 = CARTESIAN_POINT ( 'NONE',  ( -15.49969986081099727, 20.99262100756200056, 16.16206422150100153 ) ) ;
#8746 = CIRCLE ( 'NONE', #2165, 9.974999999999999645 ) ;
#8747 = CARTESIAN_POINT ( 'NONE',  ( -5.615565924346646476, -12.16405426399944112, 56.85231026484400019 ) ) ;
#8748 = ORIENTED_EDGE ( 'NONE', *, *, #10435, .T. ) ;
#8749 = CARTESIAN_POINT ( 'NONE',  ( 2.500300139188998738, -46.50737899243799944, -2.997689735156002122 ) ) ;
#8750 =( GEOMETRIC_REPRESENTATION_CONTEXT ( 3 ) GLOBAL_UNCERTAINTY_ASSIGNED_CONTEXT ( ( #14159 ) ) GLOBAL_UNIT_ASSIGNED_CONTEXT ( ( #9265, #11490, #3234 ) ) REPRESENTATION_CONTEXT ( 'NONE', 'WORKASPACE' ) );
#8751 = CARTESIAN_POINT ( 'NONE',  ( 4.905497514832876327, 5.977487861575268013, 18.88777277397837651 ) ) ;
#8752 = CARTESIAN_POINT ( 'NONE',  ( -15.49969986081099904, 22.99262100756200056, 24.21206422150100224 ) ) ;
#8753 = AXIS2_PLACEMENT_3D ( 'NONE', #7311, #1962, #12367 ) ;
#8754 = LINE ( 'NONE', #12593, #7265 ) ;
#8755 = UNCERTAINTY_MEASURE_WITH_UNIT (LENGTH_MEASURE( 1.000000000000000082E-05 ), #7393, 'distance_accuracy_value', 'NONE');
#8756 = DIRECTION ( 'NONE',  ( 0.000000000000000000, -1.000000000000000000, -1.224646799147350002E-16 ) ) ;
#8757 = EDGE_CURVE ( 'NONE', #3679, #6892, #2968, .T. ) ;
#8758 = DIRECTION ( 'NONE',  ( -8.018662683283439195E-16, 5.975035461963190001E-16, 1.000000000000000000 ) ) ;
#8759 = EDGE_LOOP ( 'NONE', ( #7178, #1006, #3561, #15089, #8415, #7212, #4312, #14824, #933 ) ) ;
#8760 = CARTESIAN_POINT ( 'NONE',  ( -7.307539508764906877, -16.04208977798462854, 56.85231026484400019 ) ) ;
#8761 = VECTOR ( 'NONE', #11182, 1000.000000000000114 ) ;
#8762 = DIRECTION ( 'NONE',  ( 0.8018662683283436232, -0.5975035461963189576, 9.999999999999996833E-16 ) ) ;
#8763 = ORIENTED_EDGE ( 'NONE', *, *, #3385, .T. ) ;
#8764 = ADVANCED_FACE ( 'NONE', ( #12235 ), #1673, .T. ) ;
#8765 = CARTESIAN_POINT ( 'NONE',  ( 21.94819177811133315, -24.42452669754511874, 26.19626277716416496 ) ) ;
#8766 = DIRECTION ( 'NONE',  ( 0.2196982563774082797, 0.9755678736739573642, -4.067366430757958773E-16 ) ) ;
#8767 = ORIENTED_EDGE ( 'NONE', *, *, #8102, .T. ) ;
#8768 = LINE ( 'NONE', #14442, #5666 ) ;
#8769 = CLOSED_SHELL ( 'NONE', ( #11863, #7431, #3172, #9036, #11684, #14118, #7167, #8532, #6020, #7620, #9087, #11398, #10278, #2521, #1593, #4213, #2591, #3249, #2210, #1027, #1963, #4023, #13461, #10356, #327, #14425, #7746, #7712, #10176, #7146, #3626, #571 ) ) ;
#8770 = DIRECTION ( 'NONE',  ( 0.000000000000000000, 1.000000000000000000, 1.224646799147350002E-16 ) ) ;
#8771 = AXIS2_PLACEMENT_3D ( 'NONE', #2162, #9182, #14782 ) ;
#8772 = EDGE_CURVE ( 'NONE', #10639, #10198, #8779, .T. ) ;
#8773 = VECTOR ( 'NONE', #3019, 1000.000000000000227 ) ;
#8774 = DIRECTION ( 'NONE',  ( 0.5975035461963189576, 0.8018662683283437342, 0.000000000000000000 ) ) ;
#8775 = CARTESIAN_POINT ( 'NONE',  ( -15.61203582816999891, -107.3496051183401647, -7.070526720097524809 ) ) ;
#8776 = EDGE_CURVE ( 'NONE', #14925, #8983, #7251, .T. ) ;
#8777 = CARTESIAN_POINT ( 'NONE',  ( -2.216578225681298697, -31.14135358865360104, -10.85656391856669778 ) ) ;
#8778 = VERTEX_POINT ( 'NONE', #12155 ) ;
#8779 = LINE ( 'NONE', #835, #9457 ) ;
#8780 = EDGE_CURVE ( 'NONE', #5861, #13533, #11661, .T. ) ;
#8781 = DIRECTION ( 'NONE',  ( 0.000000000000000000, 0.000000000000000000, -1.000000000000000000 ) ) ;
#8782 = ORIENTED_EDGE ( 'NONE', *, *, #2335, .F. ) ;
#8784 = ORIENTED_EDGE ( 'NONE', *, *, #11773, .T. ) ;
#8783 = CARTESIAN_POINT ( 'NONE',  ( -36.73657997911097794, -37.32854632934932937, -11.40473475594660968 ) ) ;
#8785 = ORIENTED_EDGE ( 'NONE', *, *, #12420, .T. ) ;
#8786 = AXIS2_PLACEMENT_3D ( 'NONE', #12666, #5688, #11655 ) ;
#8787 = CARTESIAN_POINT ( 'NONE',  ( -7.512805849530849400, -44.04964101872660365, -5.039951761444699585 ) ) ;
#8788 = DIRECTION ( 'NONE',  ( -1.000000000000000000, -3.632077277826439854E-16, 0.000000000000000000 ) ) ;
#8789 = EDGE_CURVE ( 'NONE', #12994, #1380, #8231, .T. ) ;
#8790 = LINE ( 'NONE', #7787, #8109 ) ;
#8791 = DIRECTION ( 'NONE',  ( 1.000000000000000000, 1.201369187114119994E-15, 9.616040805000176517E-16 ) ) ;
#8792 = CARTESIAN_POINT ( 'NONE',  ( -15.49969986081092088, -13.50737899243822504, 56.85231026484398598 ) ) ;
#8793 = DIRECTION ( 'NONE',  ( 0.000000000000000000, 1.000000000000000000, 1.224646799147350002E-16 ) ) ;
#8794 = CARTESIAN_POINT ( 'NONE',  ( -9.425865349984700714, -18.82901260770113794, 56.85231026484400019 ) ) ;
#8795 = EDGE_CURVE ( 'NONE', #2212, #1827, #4188, .T. ) ;
#8796 = EDGE_CURVE ( 'NONE', #14198, #10775, #12463, .T. ) ;
#8797 = DIRECTION ( 'NONE',  ( -0.8772189822852959340, 0.4800904676395371662, -9.902680687415702019E-16 ) ) ;
#8798 = ORIENTED_EDGE ( 'NONE', *, *, #5067, .F. ) ;
#8799 = DIRECTION ( 'NONE',  ( 0.8018662683283436232, -0.5975035461963189576, 9.999999999999996833E-16 ) ) ;
#8800 = VECTOR ( 'NONE', #4993, 1000.000000000000000 ) ;
#8801 = VERTEX_POINT ( 'NONE', #676 ) ;
#8802 = CARTESIAN_POINT ( 'NONE',  ( -15.53608329785963527, -13.54167542823733328, 56.85231026484398598 ) ) ;
#8804 = ORIENTED_EDGE ( 'NONE', *, *, #1496, .T. ) ;
#8803 = CARTESIAN_POINT ( 'NONE',  ( -20.65541546412893226, -22.04665423204158969, 56.85231026484398598 ) ) ;
#8805 = VERTEX_POINT ( 'NONE', #528 ) ;
#8806 = LINE ( 'NONE', #8658, #6148 ) ;
#8808 = VERTEX_POINT ( 'NONE', #5343 ) ;
#8807 = DIRECTION ( 'NONE',  ( 0.000000000000000000, -1.000000000000000000, -1.224646799147350002E-16 ) ) ;
#8809 = FACE_OUTER_BOUND ( 'NONE', #10329, .T. ) ;
#8810 = EDGE_CURVE ( 'NONE', #10889, #10559, #2825, .T. ) ;
#8811 = DIRECTION ( 'NONE',  ( 0.5975035461963188466, 0.8018662683283437342, 0.000000000000000000 ) ) ;
#8812 = CARTESIAN_POINT ( 'NONE',  ( -20.69940085690220144, -18.30574950243923027, 56.85231026484398598 ) ) ;
#8814 = FACE_OUTER_BOUND ( 'NONE', #7963, .T. ) ;
#8813 = DIRECTION ( 'NONE',  ( -8.018662683283438208E-16, 5.975035461963189015E-16, 1.000000000000000000 ) ) ;
#8815 = ORIENTED_EDGE ( 'NONE', *, *, #2316, .F. ) ;
#8816 = DIRECTION ( 'NONE',  ( 0.000000000000000000, 1.224646799147350002E-16, -1.000000000000000000 ) ) ;
#8817 = CARTESIAN_POINT ( 'NONE',  ( -21.18752042047970363, -7.775019331617081697, 57.00231026484397745 ) ) ;
#8818 = ORIENTED_EDGE ( 'NONE', *, *, #14745, .T. ) ;
#8819 = EDGE_LOOP ( 'NONE', ( #12955, #2358, #4564, #7102 ) ) ;
#8820 = CARTESIAN_POINT ( 'NONE',  ( -17.32633557924186007, -52.30049142393889383, 56.95868565438303222 ) ) ;
#8821 = VERTEX_POINT ( 'NONE', #5193 ) ;
#8822 = CARTESIAN_POINT ( 'NONE',  ( -24.08903783298838519, -16.43731469134198520, 56.85231026484398598 ) ) ;
#8823 = EDGE_CURVE ( 'NONE', #14257, #14381, #4832, .T. ) ;
#8824 = CARTESIAN_POINT ( 'NONE',  ( 13.85920135429429934, -23.75737899243800300, 5.212064221501000461 ) ) ;
#8825 = CARTESIAN_POINT ( 'NONE',  ( -15.53608329785963527, -13.54167542823733328, 56.85231026484398598 ) ) ;
#8826 = VECTOR ( 'NONE', #5138, 1000.000000000000000 ) ;
#8827 = CARTESIAN_POINT ( 'NONE',  ( 17.85205907671969783, -24.33051221079297477, 7.067054605798079869 ) ) ;
#8828 = CARTESIAN_POINT ( 'NONE',  ( -15.49969986081099904, 4.873818854045000037, 24.21206422150099868 ) ) ;
#8829 = DIRECTION ( 'NONE',  ( 0.1165201156931293391, 0.9931883319083343320, -4.999999999999998416E-16 ) ) ;
#8830 = EDGE_LOOP ( 'NONE', ( #11787, #3462, #10611, #3353 ) ) ;
#8831 = DIRECTION ( 'NONE',  ( 0.000000000000000000, 1.000000000000000000, 1.224646799147350002E-16 ) ) ;
#8832 = DIRECTION ( 'NONE',  ( 1.000000000000000000, 1.201369187114119994E-15, 9.616040805000176517E-16 ) ) ;
#8833 = VERTEX_POINT ( 'NONE', #7555 ) ;
#8834 = CARTESIAN_POINT ( 'NONE',  ( 2.112638720354275801, 8.260196310773689987, 31.34027865485604991 ) ) ;
#8835 = CIRCLE ( 'NONE', #8587, 37.50000000000000000 ) ;
#8836 = CARTESIAN_POINT ( 'NONE',  ( 21.93904460677752510, -24.55902234006768126, 26.35984492706892013 ) ) ;
#8837 = CIRCLE ( 'NONE', #10060, 9.974999999999997868 ) ;
#8838 = DIRECTION ( 'NONE',  ( -0.9354976265738682573, 0.3533329742249642913, -9.612616959383187437E-16 ) ) ;
#8839 = VERTEX_POINT ( 'NONE', #4196 ) ;
#8840 = PLANE ( 'NONE',  #1248 ) ;
#8841 = CIRCLE ( 'NONE', #13013, 0.4500000000000011768 ) ;
#8842 = PRODUCT_DEFINITION_SHAPE ( 'NONE', 'NONE',  #12004 ) ;
#8843 = VECTOR ( 'NONE', #766, 1000.000000000000000 ) ;
#8844 = ADVANCED_FACE ( 'NONE', ( #3044 ), #7699, .F. ) ;
#8845 = DIRECTION ( 'NONE',  ( -8.018662683283439195E-16, 5.975035461963190001E-16, 1.000000000000000000 ) ) ;
#8846 = CARTESIAN_POINT ( 'NONE',  ( 0.000000000000000000, 0.000000000000000000, 0.000000000000000000 ) ) ;
#8847 = EDGE_CURVE ( 'NONE', #3791, #2017, #8924, .T. ) ;
#8848 = DIRECTION ( 'NONE',  ( -1.000000000000000000, -1.201369187114119994E-15, -9.616040805000176517E-16 ) ) ;
#8849 = VECTOR ( 'NONE', #10509, 999.9999999999998863 ) ;
#8850 = VECTOR ( 'NONE', #6117, 1000.000000000000000 ) ;
#8851 = CARTESIAN_POINT ( 'NONE',  ( -7.886584594865190034, -46.96511696614950182, -7.955427708867500058 ) ) ;
#8852 = CARTESIAN_POINT ( 'NONE',  ( -18.54556661251663030, -20.98627902725976213, 56.85231026484398598 ) ) ;
#8853 = ORIENTED_EDGE ( 'NONE', *, *, #11055, .F. ) ;
#8854 = CARTESIAN_POINT ( 'NONE',  ( -15.49969986081099016, -110.5973680591374944, -10.96878667356168791 ) ) ;
#8855 = CARTESIAN_POINT ( 'NONE',  ( -7.507568439312231057, -44.88869056754154485, -3.592341908997338074 ) ) ;
#8856 = CARTESIAN_POINT ( 'NONE',  ( -20.61203582816999713, -107.3495032605914616, -7.069992522393071965 ) ) ;
#8857 = ORIENTED_EDGE ( 'NONE', *, *, #7360, .F. ) ;
#8859 = ORIENTED_EDGE ( 'NONE', *, *, #6154, .F. ) ;
#8858 = CARTESIAN_POINT ( 'NONE',  ( -15.49969986081091555, -110.0073789924380065, -5.497689735156000346 ) ) ;
#8860 = EDGE_LOOP ( 'NONE', ( #5597, #5265, #7851, #11276 ) ) ;
#8861 = DIRECTION ( 'NONE',  ( 0.7805252200231685977, -0.6251242923673534513, 9.993908270190957033E-16 ) ) ;
#8862 = CIRCLE ( 'NONE', #8129, 19.00000000000000000 ) ;
#8863 = ADVANCED_FACE ( 'NONE', ( #10307 ), #13908, .F. ) ;
#8865 = CIRCLE ( 'NONE', #4729, 5.000000000000000000 ) ;
#8864 = FACE_OUTER_BOUND ( 'NONE', #322, .T. ) ;
#8866 = ADVANCED_FACE ( 'NONE', ( #14905 ), #4501, .F. ) ;
#8867 = CARTESIAN_POINT ( 'NONE',  ( -3.499699860810999041, -57.00737899243800655, 55.03046811182510112 ) ) ;
#8868 = EDGE_CURVE ( 'NONE', #9881, #6584, #14399, .T. ) ;
#8869 = CARTESIAN_POINT ( 'NONE',  ( -8.893080693810389903, -5.970021046718354540, 61.12850859281176952 ) ) ;
#8870 = DIRECTION ( 'NONE',  ( 0.000000000000000000, 0.000000000000000000, 1.000000000000000000 ) ) ;
#8871 = CYLINDRICAL_SURFACE ( 'NONE', #14128, 9.974999999999999645 ) ;
#8872 = EDGE_CURVE ( 'NONE', #2134, #6821, #4427, .T. ) ;
#8873 = AXIS2_PLACEMENT_3D ( 'NONE', #8392, #7233, #11919 ) ;
#8874 = DIRECTION ( 'NONE',  ( 0.5975035461963188466, 0.8018662683283437342, 0.000000000000000000 ) ) ;
#8875 = ORIENTED_EDGE ( 'NONE', *, *, #12567, .T. ) ;
#8876 = CARTESIAN_POINT ( 'NONE',  ( 7.500300139189000070, -37.00737899243799944, 49.12071670408379731 ) ) ;
#8877 = DIRECTION ( 'NONE',  ( 0.2640193276336892936, -0.9645173894937585368, 7.880107536067212861E-16 ) ) ;
#8879 = VERTEX_POINT ( 'NONE', #12924 ) ;
#8878 = CARTESIAN_POINT ( 'NONE',  ( -11.58094331127308507, -5.879823872646938732, 57.00231026484397745 ) ) ;
#8880 = ORIENTED_EDGE ( 'NONE', *, *, #6521, .F. ) ;
#8881 = DIRECTION ( 'NONE',  ( 0.000000000000000000, 0.000000000000000000, 1.000000000000000000 ) ) ;
#8883 = ORIENTED_EDGE ( 'NONE', *, *, #10588, .T. ) ;
#8882 = CARTESIAN_POINT ( 'NONE',  ( 1.986653357079260385, 8.906201437978330304, 16.78046892755867958 ) ) ;
#8884 =( BOUNDED_CURVE ( )  B_SPLINE_CURVE ( 3, ( #304, #8549, #10623, #3739 ),
 .UNSPECIFIED., .F., .F. ) 
 B_SPLINE_CURVE_WITH_KNOTS ( ( 4, 4 ),
 ( 5.266983419591701576, 7.299387194767476217 ),
 .UNSPECIFIED. ) 
 CURVE ( )  GEOMETRIC_REPRESENTATION_ITEM ( )  RATIONAL_B_SPLINE_CURVE ( ( 1.000000000000000000, 0.6843990470536877035, 0.6843990470536877035, 1.000000000000000000 ) ) 
 REPRESENTATION_ITEM ( '' )  );
#8885 = CONICAL_SURFACE ( 'NONE', #2298, 23.00000000000000000, 1.047197551196598297 ) ;
#8886 = CARTESIAN_POINT ( 'NONE',  ( -10.99969986081100082, -13.21348903481619708, -13.01695671647156516 ) ) ;
#8887 = EDGE_CURVE ( 'NONE', #8293, #7892, #3878, .T. ) ;
#8888 = EDGE_CURVE ( 'NONE', #1356, #7229, #14135, .T. ) ;
#8889 = CARTESIAN_POINT ( 'NONE',  ( 0.8003001391889992266, 3.992621007561997892, 24.21206422150099868 ) ) ;
#8890 = PLANE ( 'NONE',  #8305 ) ;
#8891 =( NAMED_UNIT ( * ) PLANE_ANGLE_UNIT ( ) SI_UNIT ( $, .RADIAN. ) );
#8892 = DIRECTION ( 'NONE',  ( -0.2975196656470009415, 0.9547156899063180546, -8.090169943749472730E-16 ) ) ;
#8893 = AXIS2_PLACEMENT_3D ( 'NONE', #195, #9516, #5085 ) ;
#8894 = CARTESIAN_POINT ( 'NONE',  ( -7.016473591028808521, -8.259951331604913349, 56.85231026484400019 ) ) ;
#8895 = ORIENTED_EDGE ( 'NONE', *, *, #13359, .T. ) ;
#8896 = CARTESIAN_POINT ( 'NONE',  ( -16.48891182509095543, -11.21141303238454334, 51.00231026484399166 ) ) ;
#8897 = ORIENTED_EDGE ( 'NONE', *, *, #2672, .F. ) ;
#8898 = CARTESIAN_POINT ( 'NONE',  ( -15.49969986081086226, -13.50737899243826767, -13.99768973515600301 ) ) ;
#8899 = ORIENTED_EDGE ( 'NONE', *, *, #2335, .T. ) ;
#8900 = ORIENTED_EDGE ( 'NONE', *, *, #11496, .F. ) ;
#8901 = VECTOR ( 'NONE', #15122, 1000.000000000000000 ) ;
#8902 = DIRECTION ( 'NONE',  ( 0.000000000000000000, 1.000000000000000000, 1.224646799147350002E-16 ) ) ;
#8903 = ORIENTED_EDGE ( 'NONE', *, *, #15077, .T. ) ;
#8904 = LINE ( 'NONE', #14501, #13275 ) ;
#8905 = PLANE ( 'NONE',  #8661 ) ;
#8906 = LINE ( 'NONE', #13440, #4896 ) ;
#8907 = DIRECTION ( 'NONE',  ( -8.018662683283438208E-16, 5.975035461963189015E-16, 1.000000000000000000 ) ) ;
#8908 = PLANE ( 'NONE',  #11574 ) ;
#8910 = DIRECTION ( 'NONE',  ( -1.000000000000000000, 1.291538348938060198E-32, -1.054621095516909827E-16 ) ) ;
#8909 = FACE_OUTER_BOUND ( 'NONE', #10576, .T. ) ;
#8911 = ORIENTED_EDGE ( 'NONE', *, *, #12432, .T. ) ;
#8912 = DIRECTION ( 'NONE',  ( 1.000000000000000000, 1.201369187114119994E-15, 9.616040805000176517E-16 ) ) ;
#8913 = CARTESIAN_POINT ( 'NONE',  ( -15.49969986081099904, 70.81438635534659909, 30.46206422150100934 ) ) ;
#8914 = EDGE_CURVE ( 'NONE', #13944, #11184, #375, .T. ) ;
#8915 = ORIENTED_EDGE ( 'NONE', *, *, #2193, .T. ) ;
#8916 = CARTESIAN_POINT ( 'NONE',  ( 2.068939505948752977, 8.472784761962648403, 31.44700642079416397 ) ) ;
#8917 = EDGE_CURVE ( 'NONE', #13555, #14491, #3657, .T. ) ;
#8918 = DIRECTION ( 'NONE',  ( 1.054621095516909827E-16, 0.000000000000000000, -1.000000000000000000 ) ) ;
#8919 = CARTESIAN_POINT ( 'NONE',  ( -18.15085299098533866, -14.64962258016358554, 51.10586365543726117 ) ) ;
#8920 = DIRECTION ( 'NONE',  ( -8.018662683283439195E-16, 5.975035461963190001E-16, 1.000000000000000000 ) ) ;
#8921 = EDGE_LOOP ( 'NONE', ( #15012, #14923 ) ) ;
#8922 = DIRECTION ( 'NONE',  ( 1.000000000000000000, 1.000000000000000078E-15, 1.000000000000000078E-15 ) ) ;
#8923 = CARTESIAN_POINT ( 'NONE',  ( 2.500300139188996518, -46.50737899243799944, 44.50231026484399877 ) ) ;
#8924 = B_SPLINE_CURVE_WITH_KNOTS ( 'NONE', 3,
 ( #10385, #9154, #11609, #11458, #2054, #14825, #9079, #13684, #9306, #3348, #2204, #3279, #13830, #6774, #9230, #3199, #6852, #12690, #13980, #15048, #8158, #8001, #5714, #5561, #6702, #9004, #11382, #13757, #11533, #3501, #10234, #12537, #4653, #5857, #4574, #7927, #984, #12848, #12771, #12615, #5784, #2359, #5637 ),
 .UNSPECIFIED., .F., .F.,
 ( 4, 2, 2, 2, 2, 2, 2, 2, 2, 1, 2, 2, 2, 2, 2, 2, 2, 2, 2, 1, 1, 2, 4 ),
 ( 0.000000000000000000, 0.07105225421133361252, 0.1065783813170013972, 0.1243414448698352825, 0.1332229766462521836, 0.1421045084226690847, 0.2131567626339919419, 0.2486828897396533844, 0.2575644215160691197, 0.2664459532924848828, 0.2842090168453164090, 0.3552612710566459553, 0.3730243346094782586, 0.3819058663858942992, 0.3907873981623103399, 0.4263135252679747245, 0.4973657794793031051, 0.4995861624234071430, 0.5018065453675111254, 0.5062473112557193122, 0.5151288430321355749, 0.5328919065849679892, 0.5684180336906330400 ),
 .UNSPECIFIED. ) ;
#8925 = DIRECTION ( 'NONE',  ( -8.018662683283438208E-16, 5.975035461963189015E-16, 1.000000000000000000 ) ) ;
#8926 = DIRECTION ( 'NONE',  ( -0.5975035461963187355, -0.8018662683283439563, 0.000000000000000000 ) ) ;
#8927 = CARTESIAN_POINT ( 'NONE',  ( -12.32172653804166096, -7.186294389320899256, 56.85231026484398598 ) ) ;
#8928 = VERTEX_POINT ( 'NONE', #3802 ) ;
#8929 = DIRECTION ( 'NONE',  ( 1.000000000000000000, 1.000000000000000078E-15, 0.000000000000000000 ) ) ;
#8930 = VECTOR ( 'NONE', #10765, 1000.000000000000000 ) ;
#8931 = LINE ( 'NONE', #1980, #13877 ) ;
#8932 = EDGE_CURVE ( 'NONE', #3521, #8778, #434, .T. ) ;
#8933 = ORIENTED_EDGE ( 'NONE', *, *, #6782, .F. ) ;
#8935 = ORIENTED_EDGE ( 'NONE', *, *, #1220, .T. ) ;
#8934 = FACE_OUTER_BOUND ( 'NONE', #4385, .T. ) ;
#8936 = ORIENTED_EDGE ( 'NONE', *, *, #6429, .F. ) ;
#8937 = CARTESIAN_POINT ( 'NONE',  ( -15.49969986081093509, -96.50737899243799234, -0.1262635860074601546 ) ) ;
#8938 = CARTESIAN_POINT ( 'NONE',  ( -15.49969986081099904, -52.50737899243799944, 57.00231026484399166 ) ) ;
#8939 = DIRECTION ( 'NONE',  ( 0.000000000000000000, 1.000000000000000000, 1.224646799147350002E-16 ) ) ;
#8940 = CARTESIAN_POINT ( 'NONE',  ( -14.76203582817000104, -106.8344286703292170, -4.368659857491133280 ) ) ;
#8941 = AXIS2_PLACEMENT_3D ( 'NONE', #12326, #1843, #6488 ) ;
#8942 = DIRECTION ( 'NONE',  ( -8.018662683283438208E-16, 5.975035461963189015E-16, 1.000000000000000000 ) ) ;
#8943 = CARTESIAN_POINT ( 'NONE',  ( -21.49969986081099904, -27.00737899243800655, -5.497689735156007451 ) ) ;
#8944 = DIRECTION ( 'NONE',  ( 0.000000000000000000, -1.000000000000000000, -1.224646799147350002E-16 ) ) ;
#8945 = EDGE_CURVE ( 'NONE', #2643, #6888, #13145, .T. ) ;
#8946 = VERTEX_POINT ( 'NONE', #13150 ) ;
#8947 = LINE ( 'NONE', #10167, #10799 ) ;
#8948 = EDGE_LOOP ( 'NONE', ( #8507, #8880, #7258, #10658, #7162, #2958, #12661 ) ) ;
#8949 = VERTEX_POINT ( 'NONE', #11835 ) ;
#8950 = ORIENTED_EDGE ( 'NONE', *, *, #2351, .T. ) ;
#8951 = EDGE_CURVE ( 'NONE', #2643, #3542, #324, .T. ) ;
#8952 = CARTESIAN_POINT ( 'NONE',  ( -7.886584594865190034, -46.96511696614940234, 17.04457229113261718 ) ) ;
#8954 = EDGE_LOOP ( 'NONE', ( #605, #6408, #13989, #10191 ) ) ;
#8953 = CARTESIAN_POINT ( 'NONE',  ( -7.499699860810999041, -19.50737899243799589, 48.00231026484399877 ) ) ;
#8955 = AXIS2_PLACEMENT_3D ( 'NONE', #1168, #13872, #8121 ) ;
#8956 = DIRECTION ( 'NONE',  ( 0.000000000000000000, 1.131341397376178572E-16, -1.000000000000000000 ) ) ;
#8957 = DIRECTION ( 'NONE',  ( 8.018662683283438208E-16, -5.975035461963189015E-16, -1.000000000000000000 ) ) ;
#8958 = FACE_OUTER_BOUND ( 'NONE', #6317, .T. ) ;
#8959 = CIRCLE ( 'NONE', #2140, 10.00000000000000000 ) ;
#8960 = EDGE_CURVE ( 'NONE', #3429, #8879, #8959, .T. ) ;
#8961 = DIRECTION ( 'NONE',  ( 0.5975035461963188466, 0.8018662683283437342, 0.000000000000000000 ) ) ;
#8962 = FACE_OUTER_BOUND ( 'NONE', #7467, .T. ) ;
#8963 = EDGE_CURVE ( 'NONE', #14661, #13499, #7155, .T. ) ;
#8964 = ORIENTED_EDGE ( 'NONE', *, *, #4779, .T. ) ;
#8965 = DIRECTION ( 'NONE',  ( -1.000000000000000000, 0.000000000000000000, -0.000000000000000000 ) ) ;
#8966 = EDGE_CURVE ( 'NONE', #10775, #11940, #7131, .T. ) ;
#8967 = VERTEX_POINT ( 'NONE', #8385 ) ;
#8968 = ORIENTED_EDGE ( 'NONE', *, *, #6901, .F. ) ;
#8969 = ORIENTED_EDGE ( 'NONE', *, *, #8338, .T. ) ;
#8970 = DIRECTION ( 'NONE',  ( 0.000000000000000000, 1.000000000000000000, 1.224646799147350002E-16 ) ) ;
#8971 = ORIENTED_EDGE ( 'NONE', *, *, #14933, .F. ) ;
#8972 = AXIS2_PLACEMENT_3D ( 'NONE', #10462, #6995, #14977 ) ;
#8973 = CARTESIAN_POINT ( 'NONE',  ( -11.02342383152550553, -36.50737899243796392, 27.50231026484403074 ) ) ;
#8974 = AXIS2_PLACEMENT_3D ( 'NONE', #1198, #6003, #139 ) ;
#8975 = CARTESIAN_POINT ( 'NONE',  ( -15.49969986081091378, -13.50737899243822859, 51.00231026484399166 ) ) ;
#8976 = DIRECTION ( 'NONE',  ( -1.224646799147350002E-16, -1.224646799147350002E-16, 1.000000000000000000 ) ) ;
#8977 = CARTESIAN_POINT ( 'NONE',  ( -6.758527451665002239, -43.50737899243799944, -5.497689735156000346 ) ) ;
#8978 = VECTOR ( 'NONE', #2939, 1000.000000000000000 ) ;
#8979 = FACE_OUTER_BOUND ( 'NONE', #7648, .T. ) ;
#8981 = DIRECTION ( 'NONE',  ( -8.018662683283438208E-16, 5.975035461963189015E-16, 1.000000000000000000 ) ) ;
#8980 = LINE ( 'NONE', #14657, #13771 ) ;
#8982 = VECTOR ( 'NONE', #12361, 1000.000000000000000 ) ;
#8983 = VERTEX_POINT ( 'NONE', #13072 ) ;
#8984 = DIRECTION ( 'NONE',  ( 0.000000000000000000, -1.000000000000000000, -1.224646799147350002E-16 ) ) ;
#8985 = ADVANCED_FACE ( 'NONE', ( #11913 ), #1436, .F. ) ;
#8986 = DIRECTION ( 'NONE',  ( -0.8599296884906622029, 0.5104125104779001498, -9.945218953682734920E-16 ) ) ;
#8987 = VERTEX_POINT ( 'NONE', #14058 ) ;
#8988 = VERTEX_POINT ( 'NONE', #14288 ) ;
#8989 = DIRECTION ( 'NONE',  ( 0.000000000000000000, 0.000000000000000000, -1.000000000000000000 ) ) ;
#8990 = EDGE_CURVE ( 'NONE', #8983, #14925, #13864, .T. ) ;
#8991 = CARTESIAN_POINT ( 'NONE',  ( -17.57474910601409235, -36.77673389236314705, -17.94107779625593579 ) ) ;
#8992 = DIRECTION ( 'NONE',  ( 1.000000000000000000, 1.201369187114119994E-15, 9.616040805000176517E-16 ) ) ;
#8993 = ORIENTED_EDGE ( 'NONE', *, *, #8192, .T. ) ;
#8994 = CYLINDRICAL_SURFACE ( 'NONE', #4432, 1.074999999999999512 ) ;
#8995 =( GEOMETRIC_REPRESENTATION_CONTEXT ( 3 ) GLOBAL_UNCERTAINTY_ASSIGNED_CONTEXT ( ( #9252 ) ) GLOBAL_UNIT_ASSIGNED_CONTEXT ( ( #11714, #5890, #6040 ) ) REPRESENTATION_CONTEXT ( 'NONE', 'WORKASPACE' ) );
#8996 = CARTESIAN_POINT ( 'NONE',  ( -37.04494295528539993, 0.9926210075619987805, 16.16206422150100153 ) ) ;
#8997 = APPLICATION_PROTOCOL_DEFINITION ( 'draft international standard', 'automotive_design', 1998, #1660 ) ;
#8998 = EDGE_CURVE ( 'NONE', #9327, #14941, #6161, .T. ) ;
#8999 = CARTESIAN_POINT ( 'NONE',  ( -13.95777467540137806, -22.45074059323463089, 57.00231026484399166 ) ) ;
#9000 = AXIS2_PLACEMENT_3D ( 'NONE', #12168, #1683, #14317 ) ;
#9001 = DIRECTION ( 'NONE',  ( 1.000000000000000000, 1.201369187114119994E-15, 9.616040805000176517E-16 ) ) ;
#9002 = CARTESIAN_POINT ( 'NONE',  ( -15.49969986081099904, -57.00737899243801365, 57.00231026484399166 ) ) ;
#9003 = ORIENTED_EDGE ( 'NONE', *, *, #5579, .F. ) ;
#9004 = CARTESIAN_POINT ( 'NONE',  ( -11.50449320635804007, -90.85166671083230483, -1.907031398356576979 ) ) ;
#9005 = CARTESIAN_POINT ( 'NONE',  ( -7.508969231007553091, -44.91770256118098104, -3.568200169185395065 ) ) ;
#9006 = DIRECTION ( 'NONE',  ( -0.7109061395677416240, 0.7032868978765995926, -9.902680687415702019E-16 ) ) ;
#9007 = CLOSED_SHELL ( 'NONE', ( #5671, #9439, #11190, #13644, #406, #2897, #6804, #7553, #2932, #12104, #4435, #13123, #10723 ) ) ;
#9008 = ORIENTED_EDGE ( 'NONE', *, *, #13659, .F. ) ;
#9010 = VERTEX_POINT ( 'NONE', #5032 ) ;
#9009 = DIRECTION ( 'NONE',  ( 0.000000000000000000, -1.000000000000000000, -1.224646799147350002E-16 ) ) ;
#9011 = ORIENTED_EDGE ( 'NONE', *, *, #13728, .F. ) ;
#9012 = DIRECTION ( 'NONE',  ( 0.000000000000000000, 0.000000000000000000, 1.000000000000000000 ) ) ;
#9013 = CARTESIAN_POINT ( 'NONE',  ( -10.02412658163347636, -50.34568278964318466, 56.60086416076374860 ) ) ;
#9014 = VECTOR ( 'NONE', #3920, 999.9999999999998863 ) ;
#9015 = CARTESIAN_POINT ( 'NONE',  ( -13.81224214977857123, -23.33861042463823665, 57.00231026484399166 ) ) ;
#9016 = DIRECTION ( 'NONE',  ( -8.018662683283438208E-16, 5.975035461963189015E-16, 1.000000000000000000 ) ) ;
#9017 = EDGE_CURVE ( 'NONE', #13485, #10787, #7745, .T. ) ;
#9018 = CARTESIAN_POINT ( 'NONE',  ( -15.49969986081099904, -13.50737899243800122, 6.712064221500998684 ) ) ;
#9019 = DIRECTION ( 'NONE',  ( -2.940315329303969755E-16, 0.8386705679454240503, -0.5446390350150269732 ) ) ;
#9020 = DIRECTION ( 'NONE',  ( 0.000000000000000000, 0.000000000000000000, 1.000000000000000000 ) ) ;
#9021 = VECTOR ( 'NONE', #9994, 1000.000000000000000 ) ;
#9022 = CARTESIAN_POINT ( 'NONE',  ( -15.49969986081099904, 7.183219930803497633, 24.21206422150099868 ) ) ;
#9023 = ORIENTED_EDGE ( 'NONE', *, *, #9159, .F. ) ;
#9024 = DIRECTION ( 'NONE',  ( 0.000000000000000000, -1.000000000000000000, -1.224646799147350002E-16 ) ) ;
#9025 = CARTESIAN_POINT ( 'NONE',  ( -15.49969986081092088, -13.50737899243822504, 57.00231026484397745 ) ) ;
#9027 = ORIENTED_EDGE ( 'NONE', *, *, #6043, .T. ) ;
#9026 = CARTESIAN_POINT ( 'NONE',  ( -24.97954105023504212, -10.26796402423269150, 60.49496404811991113 ) ) ;
#9028 = B_SPLINE_CURVE_WITH_KNOTS ( 'NONE', 3,
 ( #14188, #11814, #9748, #1339, #2482, #3632 ),
 .UNSPECIFIED., .F., .F.,
 ( 4, 2, 4 ),
 ( 0.7879834095039132125, 0.8939917047519565507, 1.000000000000000000 ),
 .UNSPECIFIED. ) ;
#9029 = ORIENTED_EDGE ( 'NONE', *, *, #11717, .T. ) ;
#9030 = DIRECTION ( 'NONE',  ( -1.000000000000000000, -1.000000000000000078E-15, -1.000000000000000078E-15 ) ) ;
#9031 = DIRECTION ( 'NONE',  ( -8.018662683283438208E-16, 5.975035461963189015E-16, 1.000000000000000000 ) ) ;
#9032 = ORIENTED_EDGE ( 'NONE', *, *, #2694, .F. ) ;
#9033 = LINE ( 'NONE', #5442, #10738 ) ;
#9034 = EDGE_CURVE ( 'NONE', #13341, #1750, #14105, .T. ) ;
#9035 = DIRECTION ( 'NONE',  ( 1.000000000000000000, 1.201369187114119994E-15, 9.616040805000176517E-16 ) ) ;
#9036 = ADVANCED_FACE ( 'NONE', ( #144 ), #4804, .F. ) ;
#9037 = AXIS2_PLACEMENT_3D ( 'NONE', #5446, #11264, #12491 ) ;
#9038 = EDGE_LOOP ( 'NONE', ( #7141, #13837 ) ) ;
#9039 = CARTESIAN_POINT ( 'NONE',  ( -7.879287384819335216, -47.08648443922195526, -7.932823793481322383 ) ) ;
#9040 = PLANE ( 'NONE',  #13749 ) ;
#9041 = EDGE_LOOP ( 'NONE', ( #14309, #4834 ) ) ;
#9042 = CARTESIAN_POINT ( 'NONE',  ( 15.21167767729446396, -24.94319804950077923, 45.73146187706110055 ) ) ;
#9043 = VERTEX_POINT ( 'NONE', #4103 ) ;
#9044 = CARTESIAN_POINT ( 'NONE',  ( -28.78282149594069850, -31.14135358865360104, -10.85656391856669778 ) ) ;
#9045 = VERTEX_POINT ( 'NONE', #13593 ) ;
#9046 = ORIENTED_EDGE ( 'NONE', *, *, #13100, .T. ) ;
#9047 = CARTESIAN_POINT ( 'NONE',  ( 2.581287997393676203, -41.10853556844468670, 52.35544040764929719 ) ) ;
#9048 = ORIENTED_EDGE ( 'NONE', *, *, #12913, .F. ) ;
#9049 = CARTESIAN_POINT ( 'NONE',  ( -15.49969986081099016, -36.50737899243799944, 27.50231026484399521 ) ) ;
#9050 = ADVANCED_FACE ( 'NONE', ( #5395 ), #14835, .F. ) ;
#9051 = CARTESIAN_POINT ( 'NONE',  ( -10.15458489671155640, -90.54171561441047800, -6.038535867389205336 ) ) ;
#9052 = EDGE_CURVE ( 'NONE', #7657, #221, #6533, .T. ) ;
#9053 = CARTESIAN_POINT ( 'NONE',  ( 16.31544005195547342, -23.84671352473236183, 4.356601776764517986 ) ) ;
#9054 = EDGE_CURVE ( 'NONE', #4606, #14257, #5487, .T. ) ;
#9055 = CIRCLE ( 'NONE', #6858, 9.974999999999999645 ) ;
#9056 = CARTESIAN_POINT ( 'NONE',  ( -7.503607783881640181, -44.63988287651423548, 21.17968396569539280 ) ) ;
#9058 = CARTESIAN_POINT ( 'NONE',  ( -1.508527451664999575, -45.64135358865355130, -3.997689735156000790 ) ) ;
#9057 = DIRECTION ( 'NONE',  ( -8.018662683283438208E-16, 5.975035461963189015E-16, 1.000000000000000000 ) ) ;
#9059 = B_SPLINE_CURVE_WITH_KNOTS ( 'NONE', 3,
 ( #2184, #6680, #14883, #7978, #10052, #13888, #13664, #3099, #7758, #5470, #4407, #12511, #3329, #12440, #4331, #12669, #12596, #887, #3405, #5693 ),
 .UNSPECIFIED., .F., .F.,
 ( 4, 2, 2, 1, 1, 1, 1, 1, 1, 2, 2, 2, 4 ),
 ( 0.000000000000000000, 0.2499999999999539257, 0.3749999999999315548, 0.4374999999999203415, 0.4687499999999145128, 0.4843749999999112377, 0.4921874999999091838, 0.4960937499999086286, 0.4980468749999080735, 0.4990234374999077405, 0.4999999999999074074, 0.7499999999999538147, 1.000000000000000000 ),
 .UNSPECIFIED. ) ;
#9060 = ORIENTED_EDGE ( 'NONE', *, *, #5297, .T. ) ;
#9061 = LINE ( 'NONE', #7825, #3369 ) ;
#9062 = FACE_OUTER_BOUND ( 'NONE', #5791, .T. ) ;
#9063 = ORIENTED_EDGE ( 'NONE', *, *, #11602, .T. ) ;
#9064 = EDGE_CURVE ( 'NONE', #13179, #12486, #14513, .T. ) ;
#9065 = ORIENTED_EDGE ( 'NONE', *, *, #7217, .F. ) ;
#9066 = CYLINDRICAL_SURFACE ( 'NONE', #3239, 2.500000000000000444 ) ;
#9067 = CARTESIAN_POINT ( 'NONE',  ( -21.52722649236416430, -39.22145586813481088, -17.51198461415464180 ) ) ;
#9068 = CARTESIAN_POINT ( 'NONE',  ( -15.49969986081100082, 20.99262100756200056, 32.26206422150099939 ) ) ;
#9069 = VERTEX_POINT ( 'NONE', #8684 ) ;
#9070 = CARTESIAN_POINT ( 'NONE',  ( -15.61203582816999891, -107.9196643519486969, -5.433976602192394090 ) ) ;
#9071 = AXIS2_PLACEMENT_3D ( 'NONE', #2241, #8965, #5452 ) ;
#9072 = CARTESIAN_POINT ( 'NONE',  ( -12.04767799572592502, -20.80732214584531548, 56.85231026484400019 ) ) ;
#9073 = EDGE_CURVE ( 'NONE', #645, #1536, #13303, .T. ) ;
#9074 = CYLINDRICAL_SURFACE ( 'NONE', #6507, 4.499999999999999112 ) ;
#9075 = CARTESIAN_POINT ( 'NONE',  ( -16.91203582817000139, -107.1622034095870077, -6.087689735156001980 ) ) ;
#9076 = CARTESIAN_POINT ( 'NONE',  ( -15.19690733689918538, -23.47778227853769195, 57.00231026484399166 ) ) ;
#9077 = AXIS2_PLACEMENT_3D ( 'NONE', #10427, #7967, #9195 ) ;
#9078 = EDGE_LOOP ( 'NONE', ( #11352, #4443, #5002, #1344 ) ) ;
#9079 = CARTESIAN_POINT ( 'NONE',  ( -15.00778987199241143, -94.12399836386714469, -0.1485842411706335409 ) ) ;
#9080 = LINE ( 'NONE', #5267, #5553 ) ;
#9081 = LINE ( 'NONE', #5639, #5951 ) ;
#9082 = CONICAL_SURFACE ( 'NONE', #2492, 3.000000000000002665, 1.047197551196598297 ) ;
#9083 = VECTOR ( 'NONE', #11319, 1000.000000000000114 ) ;
#9084 = ORIENTED_EDGE ( 'NONE', *, *, #13662, .F. ) ;
#9085 = CARTESIAN_POINT ( 'NONE',  ( -7.499699860810999930, -44.62460413890913458, 46.15861046013883140 ) ) ;
#9086 = VERTEX_POINT ( 'NONE', #512 ) ;
#9087 = ADVANCED_FACE ( 'NONE', ( #5106 ), #5796, .T. ) ;
#9088 = CARTESIAN_POINT ( 'NONE',  ( -0.3742611254310274083, -27.95036676736705417, -14.90232471354687860 ) ) ;
#9089 = CARTESIAN_POINT ( 'NONE',  ( -15.49969986081100082, -110.0806363094795728, -1.108957527449961233 ) ) ;
#9090 = VECTOR ( 'NONE', #3641, 1000.000000000000000 ) ;
#9091 = CARTESIAN_POINT ( 'NONE',  ( -5.596483669297570351, -12.31283553816471432, 57.00231026484399166 ) ) ;
#9092 = CARTESIAN_POINT ( 'NONE',  ( -8.708182160528487259, -48.73602156695860543, 43.35738220827035860 ) ) ;
#9093 = VECTOR ( 'NONE', #15060, 1000.000000000000114 ) ;
#9094 = AXIS2_PLACEMENT_3D ( 'NONE', #1937, #1635, #12345 ) ;
#9095 = LINE ( 'NONE', #14839, #1875 ) ;
#9096 = CARTESIAN_POINT ( 'NONE',  ( -18.50396719079564889, -6.011671700261853601, 57.00231026484397745 ) ) ;
#9097 = PLANE ( 'NONE',  #5001 ) ;
#9098 = DIRECTION ( 'NONE',  ( -0.8660254037844387076, -0.4999999999999998890, 0.000000000000000000 ) ) ;
#9099 = VERTEX_POINT ( 'NONE', #443 ) ;
#9100 = CARTESIAN_POINT ( 'NONE',  ( 16.31615091610032309, -30.15025373772158446, 44.06283711198566522 ) ) ;
#9101 = ORIENTED_EDGE ( 'NONE', *, *, #10473, .T. ) ;
#9102 = CARTESIAN_POINT ( 'NONE',  ( -15.61203582816999891, -106.7406604375499626, -7.297873098422156701 ) ) ;
#9104 = VERTEX_POINT ( 'NONE', #9768 ) ;
#9103 = CARTESIAN_POINT ( 'NONE',  ( -24.46506769706380169, -9.065967042131633846, 60.62493186400067202 ) ) ;
#9105 = ADVANCED_FACE ( 'NONE', ( #2953 ), #2808, .T. ) ;
#9106 = ORIENTED_EDGE ( 'NONE', *, *, #5228, .F. ) ;
#9107 = EDGE_CURVE ( 'NONE', #2245, #5139, #4334, .T. ) ;
#9108 = VECTOR ( 'NONE', #11856, 1000.000000000000114 ) ;
#9109 = DIRECTION ( 'NONE',  ( 1.000000000000000000, 1.000000000000000078E-15, 0.000000000000000000 ) ) ;
#9110 = VERTEX_POINT ( 'NONE', #3952 ) ;
#9111 = DIRECTION ( 'NONE',  ( -8.018662683283439195E-16, 5.975035461963190001E-16, 1.000000000000000000 ) ) ;
#9112 = CARTESIAN_POINT ( 'NONE',  ( -20.86213698926522397, -106.5729322520875968, -5.184177647451607029 ) ) ;
#9113 =( NAMED_UNIT ( * ) PLANE_ANGLE_UNIT ( ) SI_UNIT ( $, .RADIAN. ) );
#9114 = VECTOR ( 'NONE', #7335, 1000.000000000000000 ) ;
#9115 = AXIS2_PLACEMENT_3D ( 'NONE', #3478, #4710, #6972 ) ;
#9116 = ORIENTED_EDGE ( 'NONE', *, *, #13819, .F. ) ;
#9117 = CARTESIAN_POINT ( 'NONE',  ( -23.43509953878110608, -45.55571247603148066, -17.14847601522437870 ) ) ;
#9118 = VERTEX_POINT ( 'NONE', #9843 ) ;
#9119 = CARTESIAN_POINT ( 'NONE',  ( -15.49969986081092088, -13.50737899243822504, 56.85231026484398598 ) ) ;
#9120 = ORIENTED_EDGE ( 'NONE', *, *, #6078, .F. ) ;
#9121 = ORIENTED_EDGE ( 'NONE', *, *, #1994, .F. ) ;
#9122 = ORIENTED_EDGE ( 'NONE', *, *, #9612, .F. ) ;
#9123 = EDGE_CURVE ( 'NONE', #6010, #5192, #8615, .T. ) ;
#9124 = CARTESIAN_POINT ( 'NONE',  ( -8.722797460041883610, -15.53942693735753444, 57.00231026484399166 ) ) ;
#9125 = EDGE_LOOP ( 'NONE', ( #1943, #13224, #3104, #6164 ) ) ;
#9126 = DIRECTION ( 'NONE',  ( 0.000000000000000000, 0.1872998510044759646, 0.9823027872370621028 ) ) ;
#9127 = PLANE ( 'NONE',  #4159 ) ;
#9128 = CARTESIAN_POINT ( 'NONE',  ( -10.14011164466803017, -90.54012419075833407, -5.881547205074356910 ) ) ;
#9129 = AXIS2_PLACEMENT_3D ( 'NONE', #9232, #12774, #12618 ) ;
#9130 = AXIS2_PLACEMENT_3D ( 'NONE', #11520, #3107, #6539 ) ;
#9131 = DIRECTION ( 'NONE',  ( 8.018662683283438208E-16, -5.975035461963189015E-16, -1.000000000000000000 ) ) ;
#9133 = DIRECTION ( 'NONE',  ( 0.000000000000000000, 0.000000000000000000, 1.000000000000000000 ) ) ;
#9132 = FACE_OUTER_BOUND ( 'NONE', #11540, .T. ) ;
#9134 = ORIENTED_EDGE ( 'NONE', *, *, #3434, .F. ) ;
#9135 = FACE_OUTER_BOUND ( 'NONE', #10884, .T. ) ;
#9136 = DIRECTION ( 'NONE',  ( 0.000000000000000000, -1.000000000000000000, -1.224646799147350002E-16 ) ) ;
#9137 = VERTEX_POINT ( 'NONE', #6310 ) ;
#9138 = ORIENTED_EDGE ( 'NONE', *, *, #12487, .T. ) ;
#9139 = DIRECTION ( 'NONE',  ( 0.000000000000000000, 2.220446049250313081E-16, -1.000000000000000000 ) ) ;
#9140 = EDGE_CURVE ( 'NONE', #5678, #5628, #5544, .T. ) ;
#9141 = DIRECTION ( 'NONE',  ( 0.9931883319083343320, -0.1165201156931293391, 8.660254037844387408E-16 ) ) ;
#9142 = DIRECTION ( 'NONE',  ( 1.000000000000000000, 0.000000000000000000, 0.000000000000000000 ) ) ;
#9143 = EDGE_LOOP ( 'NONE', ( #12778, #2922, #5475, #12312 ) ) ;
#9144 = DIRECTION ( 'NONE',  ( -8.018662683283438208E-16, 5.975035461963189015E-16, 1.000000000000000000 ) ) ;
#9145 = EDGE_CURVE ( 'NONE', #12780, #2678, #2878, .T. ) ;
#9146 = AXIS2_PLACEMENT_3D ( 'NONE', #9724, #6415, #1685 ) ;
#9147 = CARTESIAN_POINT ( 'NONE',  ( -15.49969986081099904, -107.1622034095870077, -6.087689735155999315 ) ) ;
#9148 = ADVANCED_FACE ( 'NONE', ( #14583 ), #6380, .T. ) ;
#9149 = ITEM_DEFINED_TRANSFORMATION ( 'NONE', 'NONE', #13904,  #6789 ) ;
#9150 = CARTESIAN_POINT ( 'NONE',  ( -18.72761429428784297, -5.025526694139714756, 57.00231026484397745 ) ) ;
#9151 = CARTESIAN_POINT ( 'NONE',  ( -13.72291223624743317, -3.691898834178107602, 56.85231026484398598 ) ) ;
#9152 = DIRECTION ( 'NONE',  ( 0.5975035461963188466, 0.8018662683283437342, 0.000000000000000000 ) ) ;
#9153 = VERTEX_POINT ( 'NONE', #9982 ) ;
#9154 = CARTESIAN_POINT ( 'NONE',  ( -15.49962021429866255, -96.00462026634728829, -0.1262635860074601823 ) ) ;
#9155 = CARTESIAN_POINT ( 'NONE',  ( -38.49964551292070070, 3.992621007561997892, 24.16206422150099442 ) ) ;
#9156 = AXIS2_PLACEMENT_3D ( 'NONE', #2593, #11923, #2668 ) ;
#9157 = EDGE_CURVE ( 'NONE', #12884, #609, #5554, .T. ) ;
#9159 = EDGE_CURVE ( 'NONE', #5814, #2590, #3025, .T. ) ;
#9158 = CARTESIAN_POINT ( 'NONE',  ( 13.85920135429429934, -27.00737899243800300, 5.212064221501000461 ) ) ;
#9160 = ORIENTED_EDGE ( 'NONE', *, *, #12366, .T. ) ;
#9161 = DIRECTION ( 'NONE',  ( -0.7805252200231699300, 0.6251242923673516749, -9.993908270190957033E-16 ) ) ;
#9162 = ORIENTED_EDGE ( 'NONE', *, *, #12717, .F. ) ;
#9163 = LINE ( 'NONE', #4362, #541 ) ;
#9164 = CARTESIAN_POINT ( 'NONE',  ( -22.64353467404651354, -6.545608444567306172, 56.85231026484398598 ) ) ;
#9165 = DIRECTION ( 'NONE',  ( 1.000000000000000000, 1.201369187114119994E-15, 9.616040805000176517E-16 ) ) ;
#9166 = DIRECTION ( 'NONE',  ( 8.018662683283438208E-16, -5.975035461963189015E-16, -1.000000000000000000 ) ) ;
#9167 = CARTESIAN_POINT ( 'NONE',  ( -7.753733168396166775, -46.50737899243799944, 42.00231026484399166 ) ) ;
#9168 = CARTESIAN_POINT ( 'NONE',  ( -15.49969986081099371, -57.00737899243799944, -17.99768973515599768 ) ) ;
#9169 = DIRECTION ( 'NONE',  ( -8.018662683283438208E-16, 5.975035461963189015E-16, 1.000000000000000000 ) ) ;
#9170 = DIRECTION ( 'NONE',  ( -8.018662683283438208E-16, 5.975035461963189015E-16, 1.000000000000000000 ) ) ;
#9171 = CARTESIAN_POINT ( 'NONE',  ( -21.18752042047970363, -7.775019331617081697, 56.85231026484398598 ) ) ;
#9172 = EDGE_LOOP ( 'NONE', ( #12412, #5643, #12468, #2683 ) ) ;
#9173 = CARTESIAN_POINT ( 'NONE',  ( 18.53245405280427960, -27.00737899243800300, 39.96206422150099513 ) ) ;
#9174 = EDGE_CURVE ( 'NONE', #8039, #7394, #9061, .T. ) ;
#9175 = ORIENTED_EDGE ( 'NONE', *, *, #12720, .T. ) ;
#9177 = ORIENTED_EDGE ( 'NONE', *, *, #8317, .T. ) ;
#9176 = DIRECTION ( 'NONE',  ( 0.000000000000000000, -1.000000000000000000, -1.224646799147350002E-16 ) ) ;
#9178 = ORIENTED_EDGE ( 'NONE', *, *, #8508, .F. ) ;
#9179 = DIRECTION ( 'NONE',  ( 0.000000000000000000, 1.000000000000000000, 1.224646799147350002E-16 ) ) ;
#9180 = ORIENTED_EDGE ( 'NONE', *, *, #10030, .T. ) ;
#9181 = AXIS2_PLACEMENT_3D ( 'NONE', #8479, #12232, #12306 ) ;
#9182 = DIRECTION ( 'NONE',  ( -0.8660254037844387076, 0.4999999999999998890, 0.000000000000000000 ) ) ;
#9183 = CARTESIAN_POINT ( 'NONE',  ( -15.61203582817000068, -105.9033823877427096, -6.327714494218207975 ) ) ;
#9184 =( NAMED_UNIT ( * ) SI_UNIT ( $, .STERADIAN. ) SOLID_ANGLE_UNIT ( ) );
#9185 = EDGE_CURVE ( 'NONE', #14032, #11333, #6907, .T. ) ;
#9186 = ORIENTED_EDGE ( 'NONE', *, *, #8490, .F. ) ;
#9187 = CARTESIAN_POINT ( 'NONE',  ( -18.80870833456381419, -51.79568668368815310, -17.85220341531665156 ) ) ;
#9188 = ORIENTED_EDGE ( 'NONE', *, *, #5188, .F. ) ;
#9189 = DIRECTION ( 'NONE',  ( 0.9755678736739583634, -0.2196982563774038943, 9.135454576426008610E-16 ) ) ;
#9190 = ORIENTED_EDGE ( 'NONE', *, *, #13751, .F. ) ;
#9191 = FACE_OUTER_BOUND ( 'NONE', #5364, .T. ) ;
#9192 = EDGE_LOOP ( 'NONE', ( #611, #7327, #12467, #12713 ) ) ;
#9193 = AXIS2_PLACEMENT_3D ( 'NONE', #1942, #11200, #10114 ) ;
#9194 = ORIENTED_EDGE ( 'NONE', *, *, #5690, .F. ) ;
#9195 = DIRECTION ( 'NONE',  ( 0.000000000000000000, 0.1872998510044759646, 0.9823027872370621028 ) ) ;
#9196 = ORIENTED_EDGE ( 'NONE', *, *, #2626, .F. ) ;
#9197 = DIRECTION ( 'NONE',  ( 1.000000000000000000, 1.201369187114119994E-15, 9.616040805000176517E-16 ) ) ;
#9198 = VECTOR ( 'NONE', #5728, 1000.000000000000000 ) ;
#9199 = SURFACE_STYLE_FILL_AREA ( #15024 ) ;
#9200 = DIRECTION ( 'NONE',  ( 0.8357240892757724637, 0.5491495666976170531, 3.420201433256690644E-16 ) ) ;
#9201 = PRESENTATION_LAYER_ASSIGNMENT (  '', '', ( #666 ) ) ;
#9202 = EDGE_CURVE ( 'NONE', #8470, #5287, #6548, .T. ) ;
#9203 = CARTESIAN_POINT ( 'NONE',  ( -7.509245100188403299, -44.92199632866380909, 21.43533231848149967 ) ) ;
#9205 = CARTESIAN_POINT ( 'NONE',  ( -17.63705083126397355, -109.2978240960466678, -1.896298140136138288 ) ) ;
#9204 = DIRECTION ( 'NONE',  ( 0.000000000000000000, 0.000000000000000000, -1.000000000000000000 ) ) ;
#9206 = VERTEX_POINT ( 'NONE', #4333 ) ;
#9207 = CARTESIAN_POINT ( 'NONE',  ( -15.49969986081099904, 9.919219809770899232, 24.21206422150099868 ) ) ;
#9208 = AXIS2_PLACEMENT_3D ( 'NONE', #7387, #2433, #11753 ) ;
#9209 = DIRECTION ( 'NONE',  ( -1.000000000000000078E-15, 1.000000000000000000, 0.000000000000000000 ) ) ;
#9210 = VERTEX_POINT ( 'NONE', #4481 ) ;
#9211 = VERTEX_POINT ( 'NONE', #9289 ) ;
#9212 = DIRECTION ( 'NONE',  ( 1.000000000000000000, 1.201369187114119994E-15, 9.616040805000176517E-16 ) ) ;
#9213 = CIRCLE ( 'NONE', #5082, 9.974999999999999645 ) ;
#9214 = CARTESIAN_POINT ( 'NONE',  ( -16.57334897777262483, -22.01522992987520766, 56.85231026484400019 ) ) ;
#9215 = CARTESIAN_POINT ( 'NONE',  ( -15.49969986081099904, -13.50737899243800122, 6.712064221500998684 ) ) ;
#9216 = ORIENTED_EDGE ( 'NONE', *, *, #10868, .F. ) ;
#9217 = DIRECTION ( 'NONE',  ( 0.5975035461963189576, 0.8018662683283437342, 0.000000000000000000 ) ) ;
#9218 = CARTESIAN_POINT ( 'NONE',  ( 13.85920135429429934, -27.00737899243800300, 5.212064221501000461 ) ) ;
#9219 = VECTOR ( 'NONE', #9392, 1000.000000000000000 ) ;
#9220 = VECTOR ( 'NONE', #7293, 1000.000000000000000 ) ;
#9221 = CONTEXT_DEPENDENT_SHAPE_REPRESENTATION ( #2733, #8718 ) ;
#9222 = EDGE_CURVE ( 'NONE', #15001, #5098, #4841, .T. ) ;
#9223 = DIRECTION ( 'NONE',  ( -8.018662683283438208E-16, 5.975035461963189015E-16, 1.000000000000000000 ) ) ;
#9224 = VECTOR ( 'NONE', #8084, 1000.000000000000000 ) ;
#9225 = CIRCLE ( 'NONE', #13880, 9.974999999999999645 ) ;
#9226 = CARTESIAN_POINT ( 'NONE',  ( -15.49969986081092088, -13.50737899243822504, 56.85231026484398598 ) ) ;
#9227 = CARTESIAN_POINT ( 'NONE',  ( -15.61203582817000068, -106.2504778273845147, -6.614114137688407169 ) ) ;
#9228 = ADVANCED_FACE ( 'NONE', ( #1961 ), #8137, .T. ) ;
#9229 = ORIENTED_EDGE ( 'NONE', *, *, #749, .T. ) ;
#9230 = CARTESIAN_POINT ( 'NONE',  ( -13.62642369053113356, -92.14448157524431338, -0.4599730570185335266 ) ) ;
#9231 = CARTESIAN_POINT ( 'NONE',  ( -5.499699860811004370, -46.50737899243799944, 47.00231026484399877 ) ) ;
#9232 = CARTESIAN_POINT ( 'NONE',  ( -15.47724068538499154, -13.46270701644446177, 56.85231026484398598 ) ) ;
#9233 = LINE ( 'NONE', #11685, #8761 ) ;
#9234 = VERTEX_POINT ( 'NONE', #11288 ) ;
#9235 = FACE_OUTER_BOUND ( 'NONE', #5560, .T. ) ;
#9236 = EDGE_LOOP ( 'NONE', ( #66, #13435, #8029, #7807 ) ) ;
#9237 = AXIS2_PLACEMENT_3D ( 'NONE', #5914, #5764, #13958 ) ;
#9238 = LINE ( 'NONE', #74, #64 ) ;
#9239 = CARTESIAN_POINT ( 'NONE',  ( -15.49969986081099904, -32.00737899243799944, 19.50231026484400232 ) ) ;
#9240 = CARTESIAN_POINT ( 'NONE',  ( -15.49969986081099904, 4.873818854045000037, 24.21206422150099868 ) ) ;
#9241 = CARTESIAN_POINT ( 'NONE',  ( -16.24681173062539230, -5.467015265965240012, 56.85231026484398598 ) ) ;
#9242 = VECTOR ( 'NONE', #8976, 1000.000000000000000 ) ;
#9243 = ADVANCED_FACE ( 'NONE', ( #13960 ), #1174, .T. ) ;
#9244 = DIRECTION ( 'NONE',  ( 0.5975035461963188466, 0.8018662683283437342, 0.000000000000000000 ) ) ;
#9245 = EDGE_CURVE ( 'NONE', #13936, #1243, #3481, .T. ) ;
#9246 = DIRECTION ( 'NONE',  ( 1.000000000000000000, 0.000000000000000000, 0.000000000000000000 ) ) ;
#9247 = EDGE_CURVE ( 'NONE', #9646, #6722, #9728, .T. ) ;
#9248 = CARTESIAN_POINT ( 'NONE',  ( -20.87112600995945755, -108.0608273576312968, -5.497689735156002122 ) ) ;
#9249 = LINE ( 'NONE', #853, #4960 ) ;
#9250 = VERTEX_POINT ( 'NONE', #1040 ) ;
#9251 = DIRECTION ( 'NONE',  ( 0.5975035461963189576, 0.8018662683283437342, 0.000000000000000000 ) ) ;
#9252 = UNCERTAINTY_MEASURE_WITH_UNIT (LENGTH_MEASURE( 1.000000000000000082E-05 ), #11714, 'distance_accuracy_value', 'NONE');
#9253 = VECTOR ( 'NONE', #5365, 1000.000000000000000 ) ;
#9254 = ORIENTED_EDGE ( 'NONE', *, *, #2818, .F. ) ;
#9256 = EDGE_LOOP ( 'NONE', ( #3659, #7064, #5680, #4910 ) ) ;
#9255 = CARTESIAN_POINT ( 'NONE',  ( -23.02173274162242578, -6.908505027013068123, 60.95052117575047390 ) ) ;
#9257 = EDGE_CURVE ( 'NONE', #11105, #3128, #8498, .T. ) ;
#9258 = ORIENTED_EDGE ( 'NONE', *, *, #7282, .F. ) ;
#9259 = PRODUCT_DEFINITION_FORMATION_WITH_SPECIFIED_SOURCE ( 'ANY', '', #7330, .NOT_KNOWN. ) ;
#9260 = DIRECTION ( 'NONE',  ( 0.000000000000000000, -1.225619847157526848E-16, 1.000000000000000000 ) ) ;
#9261 = ORIENTED_EDGE ( 'NONE', *, *, #14593, .F. ) ;
#9262 = DIRECTION ( 'NONE',  ( 0.000000000000000000, 1.000000000000000000, 1.224646799147350002E-16 ) ) ;
#9263 = CARTESIAN_POINT ( 'NONE',  ( -20.84918524500973191, -107.3388303236057624, -5.012689735156009796 ) ) ;
#9264 = CARTESIAN_POINT ( 'NONE',  ( -23.59621936791819863, -19.33378413377806027, 54.00231026484399166 ) ) ;
#9265 =( LENGTH_UNIT ( ) NAMED_UNIT ( * ) SI_UNIT ( .MILLI., .METRE. ) );
#9266 = EDGE_CURVE ( 'NONE', #2114, #1582, #5695, .T. ) ;
#9267 = ADVANCED_FACE ( 'NONE', ( #9135 ), #965, .F. ) ;
#9268 = AXIS2_PLACEMENT_3D ( 'NONE', #12042, #14705, #12187 ) ;
#9269 = AXIS2_PLACEMENT_3D ( 'NONE', #3112, #1822, #12228 ) ;
#9270 = CARTESIAN_POINT ( 'NONE',  ( -20.37445634772518233, -50.85598640664056802, -17.68005340029201022 ) ) ;
#9271 = ORIENTED_EDGE ( 'NONE', *, *, #5030, .F. ) ;
#9272 = CARTESIAN_POINT ( 'NONE',  ( -12.10759736803031039, -16.47920669945604288, -13.13479660188859199 ) ) ;
#9273 = ORIENTED_EDGE ( 'NONE', *, *, #8772, .T. ) ;
#9274 = FACE_OUTER_BOUND ( 'NONE', #10172, .T. ) ;
#9275 = VERTEX_POINT ( 'NONE', #6682 ) ;
#9276 = ORIENTED_EDGE ( 'NONE', *, *, #13201, .T. ) ;
#9277 = LINE ( 'NONE', #5830, #11038 ) ;
#9278 = VERTEX_POINT ( 'NONE', #10365 ) ;
#9279 = PRODUCT_DEFINITION ( 'UNKNOWN', '', #714, #11556 ) ;
#9281 = ADVANCED_FACE ( 'NONE', ( #15031 ), #4555, .T. ) ;
#9280 = LINE ( 'NONE', #13951, #3488 ) ;
#9282 = DIRECTION ( 'NONE',  ( 0.5975035461963188466, 0.8018662683283437342, 0.000000000000000000 ) ) ;
#9283 = DIRECTION ( 'NONE',  ( 0.5975035461963189576, 0.8018662683283437342, 0.000000000000000000 ) ) ;
#9284 = PRESENTATION_LAYER_ASSIGNMENT (  '', '', ( #741 ) ) ;
#9285 = DIRECTION ( 'NONE',  ( -1.000000000000000000, -1.156482317317871331E-15, -1.011922027653137537E-15 ) ) ;
#9287 = PLANE ( 'NONE',  #10724 ) ;
#9286 = LINE ( 'NONE', #13957, #13051 ) ;
#9288 = ORIENTED_EDGE ( 'NONE', *, *, #1602, .T. ) ;
#9289 = CARTESIAN_POINT ( 'NONE',  ( 7.000300139189000070, -19.50737899243800300, 54.21206422150100224 ) ) ;
#9290 = LINE ( 'NONE', #10519, #11812 ) ;
#9291 = ORIENTED_EDGE ( 'NONE', *, *, #9185, .T. ) ;
#9292 = ORIENTED_EDGE ( 'NONE', *, *, #4961, .T. ) ;
#9293 = FACE_OUTER_BOUND ( 'NONE', #8819, .T. ) ;
#9294 = AXIS2_PLACEMENT_3D ( 'NONE', #620, #12026, #13401 ) ;
#9295 = CARTESIAN_POINT ( 'NONE',  ( -23.49969986081100259, -44.50737899243799944, 56.13904046828872652 ) ) ;
#9296 = ORIENTED_EDGE ( 'NONE', *, *, #6896, .F. ) ;
#9297 = DIRECTION ( 'NONE',  ( 1.366025403784438385E-15, -0.8910065241883674547, -0.4539904997395473596 ) ) ;
#9298 = ORIENTED_EDGE ( 'NONE', *, *, #10357, .T. ) ;
#9299 = CARTESIAN_POINT ( 'NONE',  ( -8.791486474964740339, -6.124933722071906672, 54.00231026484399166 ) ) ;
#9300 = EDGE_CURVE ( 'NONE', #6631, #10198, #5271, .T. ) ;
#9301 = DIRECTION ( 'NONE',  ( 1.000000000000000000, 1.201369187114119994E-15, 9.616040805000176517E-16 ) ) ;
#9302 = CARTESIAN_POINT ( 'NONE',  ( 2.500300139188999182, -42.00737899243800655, 19.50231026484398811 ) ) ;
#9303 = CARTESIAN_POINT ( 'NONE',  ( -18.09969986081091875, -109.5095050892490889, -1.369115884304552999 ) ) ;
#9304 = DIRECTION ( 'NONE',  ( -0.9999272109403024578, 0.01206535623791937448, -8.090169943749475688E-16 ) ) ;
#9305 = EDGE_LOOP ( 'NONE', ( #6906, #834, #6557, #6188 ) ) ;
#9306 = CARTESIAN_POINT ( 'NONE',  ( -14.90205750506880378, -93.89666313514172202, -0.1595392253041037489 ) ) ;
#9307 = DIRECTION ( 'NONE',  ( -0.8222303661035965661, 0.5691548339926012501, -9.993908270190953088E-16 ) ) ;
#9308 = DIRECTION ( 'NONE',  ( -8.018662683283439195E-16, 5.975035461963190001E-16, 1.000000000000000000 ) ) ;
#9309 = EDGE_LOOP ( 'NONE', ( #2860, #4712 ) ) ;
#9310 = CARTESIAN_POINT ( 'NONE',  ( -15.49969986081099549, -110.3328521824327737, -5.921523074084650951 ) ) ;
#9311 = EDGE_LOOP ( 'NONE', ( #10372, #11554, #6942, #7351 ) ) ;
#9312 = PLANE ( 'NONE',  #5427 ) ;
#9313 = AXIS2_PLACEMENT_3D ( 'NONE', #3933, #14415, #8444 ) ;
#9314 = EDGE_CURVE ( 'NONE', #2588, #4531, #4867, .T. ) ;
#9315 = CARTESIAN_POINT ( 'NONE',  ( -7.495514965259227225, -43.99345095228513003, 19.65834624315599299 ) ) ;
#9316 = DIRECTION ( 'NONE',  ( 0.9225966037272106401, -0.3857661296576155863, 9.702957262759965065E-16 ) ) ;
#9317 = EDGE_CURVE ( 'NONE', #6794, #36, #6066, .T. ) ;
#9318 = DIRECTION ( 'NONE',  ( -1.734723475976808080E-16, 0.000000000000000000, 1.000000000000000000 ) ) ;
#9319 = CARTESIAN_POINT ( 'NONE',  ( -8.123614162940384631, -47.60880580837400800, 46.75233648801069819 ) ) ;
#9320 = DIRECTION ( 'NONE',  ( 0.2872152572324145892, 0.9578660637129379207, -3.420201433256678811E-16 ) ) ;
#9321 = AXIS2_PLACEMENT_3D ( 'NONE', #4718, #14351, #9526 ) ;
#9322 = AXIS2_PLACEMENT_3D ( 'NONE', #8560, #3029, #3822 ) ;
#9323 = CARTESIAN_POINT ( 'NONE',  ( -15.49969986081100259, -19.50737899243800300, 51.00231026484400587 ) ) ;
#9324 = CARTESIAN_POINT ( 'NONE',  ( -7.752363797594655992, -48.01475789269080252, -7.497332716824399057 ) ) ;
#9325 = CARTESIAN_POINT ( 'NONE',  ( -36.84926662630419969, -37.28744580235390771, 50.33162166081972089 ) ) ;
#9326 = DIRECTION ( 'NONE',  ( -0.9868311969055005850, -0.1617534816134010012, -6.946583704589984503E-16 ) ) ;
#9327 = VERTEX_POINT ( 'NONE', #12901 ) ;
#9328 = DIRECTION ( 'NONE',  ( 0.5975035461963189576, 0.8018662683283437342, 0.000000000000000000 ) ) ;
#9329 = VERTEX_POINT ( 'NONE', #3636 ) ;
#9331 = ORIENTED_EDGE ( 'NONE', *, *, #1377, .F. ) ;
#9330 = CARTESIAN_POINT ( 'NONE',  ( -24.15923398760522645, -8.493147050648126140, 60.69887305834505753 ) ) ;
#9332 = VERTEX_POINT ( 'NONE', #8447 ) ;
#9333 = EDGE_CURVE ( 'NONE', #8707, #13092, #14346, .T. ) ;
#9334 = CIRCLE ( 'NONE', #8605, 9.974999999999999645 ) ;
#9335 = LINE ( 'NONE', #6035, #12908 ) ;
#9336 = ADVANCED_FACE ( 'NONE', ( #5840 ), #3711, .F. ) ;
#9337 = ORIENTED_EDGE ( 'NONE', *, *, #4232, .T. ) ;
#9338 = VECTOR ( 'NONE', #728, 1000.000000000000000 ) ;
#9339 = VECTOR ( 'NONE', #13964, 1000.000000000000000 ) ;
#9340 = CARTESIAN_POINT ( 'NONE',  ( -15.09158957740191909, -106.8625236479798843, -4.516005275576694622 ) ) ;
#9341 = VECTOR ( 'NONE', #10158, 1000.000000000000000 ) ;
#9342 = EDGE_CURVE ( 'NONE', #12721, #3694, #11660, .T. ) ;
#9343 = FACE_OUTER_BOUND ( 'NONE', #14566, .T. ) ;
#9344 = DIRECTION ( 'NONE',  ( -1.000000000000000000, 0.000000000000000000, -1.011922027653137537E-15 ) ) ;
#9345 = CARTESIAN_POINT ( 'NONE',  ( 0.000000000000000000, 0.000000000000000000, 0.000000000000000000 ) ) ;
#9346 = EDGE_CURVE ( 'NONE', #17, #3306, #13133, .T. ) ;
#9347 = CARTESIAN_POINT ( 'NONE',  ( -9.002116193859002635, -10.70790913352571927, 57.00231026484399166 ) ) ;
#9348 = DIRECTION ( 'NONE',  ( 0.9885168150181788960, -0.1511109077013150503, 8.829475928589270966E-16 ) ) ;
#9349 = VECTOR ( 'NONE', #2168, 1000.000000000000000 ) ;
#9350 = DIRECTION ( 'NONE',  ( -0.5975035461963188466, -0.8018662683283437342, 0.000000000000000000 ) ) ;
#9351 = ORIENTED_EDGE ( 'NONE', *, *, #8439, .F. ) ;
#9352 = CARTESIAN_POINT ( 'NONE',  ( 6.481863649926076221, -37.10904096101434391, -10.88012559947874891 ) ) ;
#9353 = ORIENTED_EDGE ( 'NONE', *, *, #7816, .F. ) ;
#9354 = DIRECTION ( 'NONE',  ( -0.8719950447285834683, -0.4895147004624025855, -4.067366430758019910E-16 ) ) ;
#9355 = ORIENTED_EDGE ( 'NONE', *, *, #13810, .T. ) ;
#9356 = ORIENTED_EDGE ( 'NONE', *, *, #6967, .T. ) ;
#9357 = EDGE_CURVE ( 'NONE', #6428, #2864, #13330, .T. ) ;
#9358 = DIRECTION ( 'NONE',  ( -0.5691548339926102429, -0.8222303661035904598, 3.489949670250058899E-17 ) ) ;
#9359 = EDGE_CURVE ( 'NONE', #3205, #11477, #13056, .T. ) ;
#9360 = ORIENTED_EDGE ( 'NONE', *, *, #2120, .F. ) ;
#9361 = DIRECTION ( 'NONE',  ( 0.01206535623791937274, 0.9999272109403024578, -5.877852522924727828E-16 ) ) ;
#9362 = ADVANCED_BREP_SHAPE_REPRESENTATION ( '', ( #2648, #6789 ), #4119 ) ;
#9363 = VECTOR ( 'NONE', #14420, 999.9999999999998863 ) ;
#9364 = CIRCLE ( 'NONE', #3006, 23.00000000000000000 ) ;
#9365 = CARTESIAN_POINT ( 'NONE',  ( -15.49969986081099904, -36.50737899243799944, -13.49768973515600479 ) ) ;
#9366 = CARTESIAN_POINT ( 'NONE',  ( -16.91203582817000139, -107.1622034095870077, -6.087689735156001980 ) ) ;
#9367 = AXIS2_PLACEMENT_3D ( 'NONE', #8539, #11833, #2498 ) ;
#9368 = LINE ( 'NONE', #13886, #7420 ) ;
#9370 = CARTESIAN_POINT ( 'NONE',  ( -13.81224214977857123, -23.33861042463823665, 54.00231026484399166 ) ) ;
#9369 = LINE ( 'NONE', #3328, #8631 ) ;
#9371 = ORIENTED_EDGE ( 'NONE', *, *, #8170, .T. ) ;
#9372 = CARTESIAN_POINT ( 'NONE',  ( -19.55678615628314532, -20.48959216528617233, 56.85231026484398598 ) ) ;
#9373 = CARTESIAN_POINT ( 'NONE',  ( -31.79969986081099975, 11.99262100756199878, 24.26206422150100650 ) ) ;
#9374 = VERTEX_POINT ( 'NONE', #1493 ) ;
#9375 = EDGE_LOOP ( 'NONE', ( #3757, #4229, #3942, #7337 ) ) ;
#9376 = PLANE ( 'NONE',  #10564 ) ;
#9377 = VECTOR ( 'NONE', #1515, 1000.000000000000000 ) ;
#9378 = CARTESIAN_POINT ( 'NONE',  ( -17.58100468212644429, -36.76477499413114458, 56.94810725308578014 ) ) ;
#9379 = EDGE_LOOP ( 'NONE', ( #3142, #241, #1172, #7824 ) ) ;
#9380 = CARTESIAN_POINT ( 'NONE',  ( -16.58746603607634995, -23.42289157363888208, 56.85231026484400019 ) ) ;
#9381 = ORIENTED_EDGE ( 'NONE', *, *, #9809, .F. ) ;
#9382 = EDGE_CURVE ( 'NONE', #12036, #7447, #4346, .T. ) ;
#9383 = AXIS2_PLACEMENT_3D ( 'NONE', #8287, #12978, #7136 ) ;
#9384 = DIRECTION ( 'NONE',  ( -1.000000000000000000, 0.000000000000000000, 0.000000000000000000 ) ) ;
#9385 = VECTOR ( 'NONE', #11003, 1000.000000000000000 ) ;
#9386 = EDGE_CURVE ( 'NONE', #12018, #551, #4938, .T. ) ;
#9387 = EDGE_CURVE ( 'NONE', #9600, #14274, #7213, .T. ) ;
#9388 = DIRECTION ( 'NONE',  ( 0.5491495666976171641, -0.8357240892757725748, 9.396926207859082113E-16 ) ) ;
#9389 = CYLINDRICAL_SURFACE ( 'NONE', #14740, 0.2500000000000014433 ) ;
#9390 = EDGE_LOOP ( 'NONE', ( #6666, #14999, #12756, #7022, #12056, #8094 ) ) ;
#9391 = CARTESIAN_POINT ( 'NONE',  ( -2.716578225681299141, -32.00737899243799944, 54.75627176226269199 ) ) ;
#9392 = DIRECTION ( 'NONE',  ( -5.000000000000000389E-16, 0.4999999999999998890, -0.8660254037844387076 ) ) ;
#9393 = ORIENTED_EDGE ( 'NONE', *, *, #12920, .F. ) ;
#9394 = FACE_BOUND ( 'NONE', #13352, .T. ) ;
#9395 = ORIENTED_EDGE ( 'NONE', *, *, #9245, .T. ) ;
#9396 = CARTESIAN_POINT ( 'NONE',  ( -12.84854673063649422, -12.36513540471287342, 51.10586365543726117 ) ) ;
#9397 = ORIENTED_EDGE ( 'NONE', *, *, #1121, .T. ) ;
#9398 = FACE_OUTER_BOUND ( 'NONE', #6977, .T. ) ;
#9399 = DIRECTION ( 'NONE',  ( 1.000000000000000000, 0.000000000000000000, 0.000000000000000000 ) ) ;
#9400 = DIRECTION ( 'NONE',  ( 0.000000000000000000, 0.000000000000000000, 1.000000000000000000 ) ) ;
#9401 = CARTESIAN_POINT ( 'NONE',  ( -15.49969986081092088, -13.50737899243822504, 56.85231026484398598 ) ) ;
#9402 = CARTESIAN_POINT ( 'NONE',  ( -5.500669204425239656, -13.50739036851649466, 60.35526053768147392 ) ) ;
#9403 = VECTOR ( 'NONE', #11414, 1000.000000000000000 ) ;
#9404 = EDGE_CURVE ( 'NONE', #7427, #11933, #3611, .T. ) ;
#9405 = PLANE ( 'NONE',  #1622 ) ;
#9406 = CARTESIAN_POINT ( 'NONE',  ( -7.799975386333926508, -47.73689692355252134, -7.674474215535603605 ) ) ;
#9407 = DIRECTION ( 'NONE',  ( 0.5975035461963187355, 0.8018662683283439563, 0.000000000000000000 ) ) ;
#9408 = CARTESIAN_POINT ( 'NONE',  ( -12.11547932532413263, -20.83938426843124603, 56.85231026484400019 ) ) ;
#9409 = ORIENTED_EDGE ( 'NONE', *, *, #2149, .F. ) ;
#9410 = PLANE ( 'NONE',  #13003 ) ;
#9411 = ORIENTED_EDGE ( 'NONE', *, *, #14845, .T. ) ;
#9413 = ORIENTED_EDGE ( 'NONE', *, *, #13313, .F. ) ;
#9412 = FACE_OUTER_BOUND ( 'NONE', #3024, .T. ) ;
#9414 = EDGE_LOOP ( 'NONE', ( #1925, #4083, #15108, #1589, #4131 ) ) ;
#9415 = DIRECTION ( 'NONE',  ( -1.224646799147350002E-16, 0.000000000000000000, 1.000000000000000000 ) ) ;
#9416 = ORIENTED_EDGE ( 'NONE', *, *, #3457, .T. ) ;
#9417 = LINE ( 'NONE', #7106, #9500 ) ;
#9418 = DIRECTION ( 'NONE',  ( 1.000000000000000000, 1.201369187114119994E-15, 9.616040805000176517E-16 ) ) ;
#9419 = CARTESIAN_POINT ( 'NONE',  ( 2.500300139188999182, -37.00737899243799944, -13.39525803434800011 ) ) ;
#9420 = DIRECTION ( 'NONE',  ( 1.000000000000000000, 0.000000000000000000, 0.000000000000000000 ) ) ;
#9421 = CARTESIAN_POINT ( 'NONE',  ( -16.08946529960249450, -9.036566988620739593, -13.28440143531883244 ) ) ;
#9422 = ADVANCED_FACE ( 'NONE', ( #9598 ), #4713, .F. ) ;
#9423 = FACE_OUTER_BOUND ( 'NONE', #514, .T. ) ;
#9424 = DIRECTION ( 'NONE',  ( -0.9731439732146150989, -0.2301973227387161258, -6.427876096865397836E-16 ) ) ;
#9425 = ADVANCED_FACE ( 'NONE', ( #1258 ), #4788, .F. ) ;
#9426 = ORIENTED_EDGE ( 'NONE', *, *, #1484, .F. ) ;
#9427 = CARTESIAN_POINT ( 'NONE',  ( 2.708095644062286311, -40.57968410433875306, -13.28071779296938004 ) ) ;
#9428 = ORIENTED_EDGE ( 'NONE', *, *, #14355, .F. ) ;
#9429 = AXIS2_PLACEMENT_3D ( 'NONE', #10231, #10458, #7923 ) ;
#9430 = ORIENTED_EDGE ( 'NONE', *, *, #3266, .F. ) ;
#9431 = VERTEX_POINT ( 'NONE', #9445 ) ;
#9432 = DIRECTION ( 'NONE',  ( 1.000000000000000000, 1.000000000000000078E-15, 0.000000000000000000 ) ) ;
#9433 = CARTESIAN_POINT ( 'NONE',  ( 2.919159964955403197, -40.00214821739496074, 52.16723540061214237 ) ) ;
#9434 = VERTEX_POINT ( 'NONE', #14113 ) ;
#9435 = DIRECTION ( 'NONE',  ( -8.018662683283438208E-16, 5.975035461963189015E-16, 1.000000000000000000 ) ) ;
#9436 = CARTESIAN_POINT ( 'NONE',  ( -15.49969986081099904, -27.00737899243800300, 19.50231026484400587 ) ) ;
#9437 = CARTESIAN_POINT ( 'NONE',  ( -12.10298406914416525, -91.10791589579226013, -9.660565934256062803 ) ) ;
#9438 = AXIS2_PLACEMENT_3D ( 'NONE', #1072, #2299, #4822 ) ;
#9439 = ADVANCED_FACE ( 'NONE', ( #8289 ), #680, .F. ) ;
#9440 = EDGE_CURVE ( 'NONE', #13375, #7843, #13637, .T. ) ;
#9441 = CARTESIAN_POINT ( 'NONE',  ( 2.374542637206501272, 7.183219930803497633, 30.65500261342018007 ) ) ;
#9443 = DIRECTION ( 'NONE',  ( 1.054621095516909827E-16, -1.224646799147350002E-16, 1.000000000000000000 ) ) ;
#9442 = CARTESIAN_POINT ( 'NONE',  ( -7.886584594865180264, -46.96511696614940234, -3.039951761444701361 ) ) ;
#9444 = EDGE_LOOP ( 'NONE', ( #10676, #10866, #2118, #2487 ) ) ;
#9445 = CARTESIAN_POINT ( 'NONE',  ( -14.61203582817000246, -106.2504437127206529, -5.561324420954689707 ) ) ;
#9446 = CARTESIAN_POINT ( 'NONE',  ( -15.49969986081099904, 64.39262100756199914, 24.21206422150100579 ) ) ;
#9447 = ORIENTED_EDGE ( 'NONE', *, *, #9386, .T. ) ;
#9448 = EDGE_LOOP ( 'NONE', ( #10711, #7702, #13041, #2661 ) ) ;
#9449 = LINE ( 'NONE', #14122, #2745 ) ;
#9450 = VERTEX_POINT ( 'NONE', #14191 ) ;
#9451 = COLOUR_RGB ( '', 0.66274510, 0.83137255, 0.94901961) ;
#9452 = CARTESIAN_POINT ( 'NONE',  ( 7.499553822109690238, 3.992621007562000557, 24.58036929630707590 ) ) ;
#9453 = AXIS2_PLACEMENT_3D ( 'NONE', #11535, #1057, #9307 ) ;
#9454 = LINE ( 'NONE', #210, #11667 ) ;
#9455 = ADVANCED_FACE ( 'NONE', ( #8521 ), #12275, .T. ) ;
#9456 = ADVANCED_FACE ( 'NONE', ( #5380 ), #4081, .T. ) ;
#9457 = VECTOR ( 'NONE', #12383, 1000.000000000000000 ) ;
#9458 = CARTESIAN_POINT ( 'NONE',  ( -5.499699860810999041, -13.50737899243800122, 6.712064221500998684 ) ) ;
#9459 = DIRECTION ( 'NONE',  ( -1.000000000000000000, -1.000000000000000078E-15, -1.000000000000000078E-15 ) ) ;
#9460 = ORIENTED_EDGE ( 'NONE', *, *, #10527, .T. ) ;
#9461 = DIRECTION ( 'NONE',  ( -8.018662683283438208E-16, 5.975035461963189015E-16, 1.000000000000000000 ) ) ;
#9462 = CARTESIAN_POINT ( 'NONE',  ( -35.84653069491783839, 6.005480809360966177, 29.56784677734614064 ) ) ;
#9463 = ORIENTED_EDGE ( 'NONE', *, *, #13561, .F. ) ;
#9464 = DIRECTION ( 'NONE',  ( 0.000000000000000000, 2.168404344971008868E-16, -1.000000000000000000 ) ) ;
#9465 = ORIENTED_EDGE ( 'NONE', *, *, #3225, .F. ) ;
#9466 = DIRECTION ( 'NONE',  ( 8.018662683283438208E-16, -5.975035461963189015E-16, -1.000000000000000000 ) ) ;
#9467 = EDGE_LOOP ( 'NONE', ( #6050, #12579, #9586, #184 ) ) ;
#9468 = FACE_BOUND ( 'NONE', #9041, .T. ) ;
#9469 = CARTESIAN_POINT ( 'NONE',  ( -15.61203582816999891, -106.6563755045979605, -6.855836844165477117 ) ) ;
#9470 = DIRECTION ( 'NONE',  ( 1.000000000000000000, 1.000000000000000078E-15, 1.000000000000000078E-15 ) ) ;
#9471 = AXIS2_PLACEMENT_3D ( 'NONE', #607, #7929, #10003 ) ;
#9472 = AXIS2_PLACEMENT_3D ( 'NONE', #12980, #7138, #1342 ) ;
#9473 = PRODUCT_DEFINITION ( 'UNKNOWN', '', #12686, #8179 ) ;
#9474 = EDGE_CURVE ( 'NONE', #1679, #7202, #5235, .T. ) ;
#9475 = VECTOR ( 'NONE', #12919, 1000.000000000000000 ) ;
#9476 = DIRECTION ( 'NONE',  ( -1.000000000000000078E-15, 1.000000000000000000, 0.000000000000000000 ) ) ;
#9477 = FACE_OUTER_BOUND ( 'NONE', #11780, .T. ) ;
#9478 = APPLICATION_CONTEXT ( 'automotive_design' ) ;
#9479 = DIRECTION ( 'NONE',  ( 0.000000000000000000, 1.224646799147350002E-16, -1.000000000000000000 ) ) ;
#9480 = ORIENTED_EDGE ( 'NONE', *, *, #136, .T. ) ;
#9481 = CARTESIAN_POINT ( 'NONE',  ( -13.42276483944220189, -52.23752306156875136, -17.94097413569642185 ) ) ;
#9482 = AXIS2_PLACEMENT_3D ( 'NONE', #13849, #9170, #9407 ) ;
#9483 = CARTESIAN_POINT ( 'NONE',  ( -35.79116231783276447, -37.80121036461405026, 51.03851805053808732 ) ) ;
#9484 = PLANE ( 'NONE',  #12551 ) ;
#9485 = AXIS2_PLACEMENT_3D ( 'NONE', #3357, #10317, #5350 ) ;
#9486 = ORIENTED_EDGE ( 'NONE', *, *, #12311, .F. ) ;
#9487 = FACE_OUTER_BOUND ( 'NONE', #12640, .T. ) ;
#9488 = ORIENTED_EDGE ( 'NONE', *, *, #8789, .F. ) ;
#9490 = VERTEX_POINT ( 'NONE', #10900 ) ;
#9489 = PLANE ( 'NONE',  #9856 ) ;
#9491 = ORIENTED_EDGE ( 'NONE', *, *, #2608, .F. ) ;
#9492 = FACE_OUTER_BOUND ( 'NONE', #10115, .T. ) ;
#9493 = VERTEX_POINT ( 'NONE', #9897 ) ;
#9494 = AXIS2_PLACEMENT_3D ( 'NONE', #8441, #11810, #192 ) ;
#9495 = EDGE_CURVE ( 'NONE', #276, #7470, #1386, .T. ) ;
#9496 = LINE ( 'NONE', #4684, #7931 ) ;
#9497 = VECTOR ( 'NONE', #8986, 1000.000000000000114 ) ;
#9498 = LINE ( 'NONE', #14171, #10767 ) ;
#9499 = CARTESIAN_POINT ( 'NONE',  ( -19.99969986081099549, -13.20997340667671160, -13.01695671647154562 ) ) ;
#9500 = VECTOR ( 'NONE', #9262, 1000.000000000000000 ) ;
#9501 = LINE ( 'NONE', #1471, #8850 ) ;
#9502 = ORIENTED_EDGE ( 'NONE', *, *, #9743, .F. ) ;
#9503 = CARTESIAN_POINT ( 'NONE',  ( -11.59602743870534347, -15.76507124608116150, -13.08455929840592269 ) ) ;
#9504 = ORIENTED_EDGE ( 'NONE', *, *, #1013, .F. ) ;
#9505 = EDGE_LOOP ( 'NONE', ( #7043, #4777 ) ) ;
#9506 = ORIENTED_EDGE ( 'NONE', *, *, #1401, .F. ) ;
#9507 = LINE ( 'NONE', #14181, #9577 ) ;
#9508 = ORIENTED_EDGE ( 'NONE', *, *, #4839, .T. ) ;
#9509 = PLANE ( 'NONE',  #4720 ) ;
#9510 = ADVANCED_FACE ( 'NONE', ( #13282 ), #2789, .F. ) ;
#9511 = VECTOR ( 'NONE', #9741, 1000.000000000000000 ) ;
#9512 = VECTOR ( 'NONE', #2652, 1000.000000000000000 ) ;
#9513 = EDGE_CURVE ( 'NONE', #2844, #10757, #6513, .T. ) ;
#9514 = CARTESIAN_POINT ( 'NONE',  ( -14.76203582817000104, -107.1622034095870077, -6.087689735155999315 ) ) ;
#9515 = PLANE ( 'NONE',  #1196 ) ;
#9516 = DIRECTION ( 'NONE',  ( -8.018662683283438208E-16, 5.975035461963189015E-16, 1.000000000000000000 ) ) ;
#9518 = DIRECTION ( 'NONE',  ( 0.000000000000000000, -1.000000000000000000, -1.224646799147350002E-16 ) ) ;
#9517 = CARTESIAN_POINT ( 'NONE',  ( -7.501378586840250939, -49.00244658604244563, -5.658025522608453706 ) ) ;
#9519 = EDGE_LOOP ( 'NONE', ( #11312, #12164, #14622, #4888 ) ) ;
#9520 = DIRECTION ( 'NONE',  ( 1.000000000000000000, 3.700743415417188632E-16, 0.000000000000000000 ) ) ;
#9521 = CARTESIAN_POINT ( 'NONE',  ( -24.89997498294686196, -16.92210204874093549, 60.51485643764996780 ) ) ;
#9522 = ORIENTED_EDGE ( 'NONE', *, *, #12174, .T. ) ;
#9523 = VECTOR ( 'NONE', #6674, 1000.000000000000227 ) ;
#9524 = ORIENTED_EDGE ( 'NONE', *, *, #3185, .F. ) ;
#9525 = CARTESIAN_POINT ( 'NONE',  ( 21.91156137581363694, -28.99392143964606205, 26.79309724432473416 ) ) ;
#9526 = DIRECTION ( 'NONE',  ( 1.054621095516909827E-16, 0.000000000000000000, -1.000000000000000000 ) ) ;
#9527 = ORIENTED_EDGE ( 'NONE', *, *, #7076, .T. ) ;
#9528 = PLANE ( 'NONE',  #6197 ) ;
#9529 = EDGE_CURVE ( 'NONE', #7124, #11066, #6295, .T. ) ;
#9530 = VECTOR ( 'NONE', #6808, 1000.000000000000000 ) ;
#9531 = EDGE_CURVE ( 'NONE', #6280, #13533, #7444, .T. ) ;
#9532 = EDGE_CURVE ( 'NONE', #8833, #5844, #11124, .T. ) ;
#9533 = DIRECTION ( 'NONE',  ( 8.018662683283438208E-16, -5.975035461963189015E-16, -1.000000000000000000 ) ) ;
#9534 = EDGE_CURVE ( 'NONE', #9709, #560, #643, .T. ) ;
#9535 = CARTESIAN_POINT ( 'NONE',  ( -7.661865618943386913, -46.13483245617170780, 17.00230869392893496 ) ) ;
#9536 = DIRECTION ( 'NONE',  ( -1.000000000000000000, 0.000000000000000000, 0.000000000000000000 ) ) ;
#9538 = ORIENTED_EDGE ( 'NONE', *, *, #9704, .F. ) ;
#9537 = CIRCLE ( 'NONE', #6593, 4.499999999999999112 ) ;
#9539 = CARTESIAN_POINT ( 'NONE',  ( 1.872105016583413661, -24.05954647699556048, 52.82914930240929863 ) ) ;
#9540 = DIRECTION ( 'NONE',  ( 1.000000000000000000, -1.499759782661860071E-32, 1.224646799147350002E-16 ) ) ;
#9541 = VERTEX_POINT ( 'NONE', #12122 ) ;
#9542 = DIRECTION ( 'NONE',  ( 0.000000000000000000, -1.000000000000000000, -1.224646799147350002E-16 ) ) ;
#9543 = SURFACE_SIDE_STYLE ('',( #2663 ) ) ;
#9544 = VERTEX_POINT ( 'NONE', #5305 ) ;
#9545 = CARTESIAN_POINT ( 'NONE',  ( -10.99969986081099904, -13.50737899243800122, -13.01695671647155983 ) ) ;
#9546 = ORIENTED_EDGE ( 'NONE', *, *, #11443, .T. ) ;
#9547 = CARTESIAN_POINT ( 'NONE',  ( -7.754798889200088752, -46.50763646577239285, -7.996864293225370623 ) ) ;
#9548 = EDGE_CURVE ( 'NONE', #13197, #8821, #10939, .T. ) ;
#9549 = CARTESIAN_POINT ( 'NONE',  ( -15.49969986081099904, -27.00737899243800300, -5.497689735156002122 ) ) ;
#9550 = PLANE ( 'NONE',  #10812 ) ;
#9551 = CARTESIAN_POINT ( 'NONE',  ( -22.56723502526082470, -13.84084068328822070, 57.00231026484397745 ) ) ;
#9552 = DIRECTION ( 'NONE',  ( 0.6334982226805337957, -0.7737441449604673949, 9.702957262759957177E-16 ) ) ;
#9553 = CARTESIAN_POINT ( 'NONE',  ( 2.500300139188999182, -37.00737899243799944, 52.39987856403599409 ) ) ;
#9554 = ORIENTED_EDGE ( 'NONE', *, *, #14708, .F. ) ;
#9555 = CARTESIAN_POINT ( 'NONE',  ( -14.97606084353312639, -52.50737899243799234, -17.99768973515599413 ) ) ;
#9556 = CARTESIAN_POINT ( 'NONE',  ( -33.70749536570576765, -40.57968410429901951, 52.28533832264545822 ) ) ;
#9557 = AXIS2_PLACEMENT_3D ( 'NONE', #5015, #12977, #5990 ) ;
#9558 = ADVANCED_FACE ( 'NONE', ( #9965 ), #14640, .T. ) ;
#9559 = DIRECTION ( 'NONE',  ( 0.000000000000000000, -1.000000000000000000, -1.224646799147350002E-16 ) ) ;
#9560 = ORIENTED_EDGE ( 'NONE', *, *, #12998, .T. ) ;
#9561 = CARTESIAN_POINT ( 'NONE',  ( 7.500245791298697284, 3.992621007561997892, 24.16206422150099442 ) ) ;
#9562 = ORIENTED_EDGE ( 'NONE', *, *, #12253, .F. ) ;
#9564 = ORIENTED_EDGE ( 'NONE', *, *, #5100, .T. ) ;
#9563 = DIRECTION ( 'NONE',  ( -1.000000000000000000, -1.201369187114119994E-15, -9.616040805000176517E-16 ) ) ;
#9565 = ORIENTED_EDGE ( 'NONE', *, *, #10656, .T. ) ;
#9566 = CARTESIAN_POINT ( 'NONE',  ( -12.25471857405102405, -7.219983152459794162, 56.85231026484398598 ) ) ;
#9567 = VERTEX_POINT ( 'NONE', #5153 ) ;
#9568 = LINE ( 'NONE', #3606, #11704 ) ;
#9569 = FACE_OUTER_BOUND ( 'NONE', #3858, .T. ) ;
#9570 = VECTOR ( 'NONE', #13408, 1000.000000000000000 ) ;
#9571 = DIRECTION ( 'NONE',  ( 0.000000000000000000, 1.000000000000000000, 1.224646799147350002E-16 ) ) ;
#9572 = DIRECTION ( 'NONE',  ( 1.000000000000000222, 3.473783760643556207E-16, -8.049116928532384918E-16 ) ) ;
#9573 = LINE ( 'NONE', #9347, #2408 ) ;
#9574 = EDGE_CURVE ( 'NONE', #2509, #1356, #5804, .T. ) ;
#9575 = EDGE_CURVE ( 'NONE', #8805, #947, #8668, .T. ) ;
#9576 = CARTESIAN_POINT ( 'NONE',  ( -17.54662770128649285, -5.179934221328323929, 56.85231026484398598 ) ) ;
#9577 = VECTOR ( 'NONE', #4776, 1000.000000000000114 ) ;
#9578 = LINE ( 'NONE', #3769, #4933 ) ;
#9579 = ORIENTED_EDGE ( 'NONE', *, *, #7572, .T. ) ;
#9580 =( LENGTH_UNIT ( ) NAMED_UNIT ( * ) SI_UNIT ( .MILLI., .METRE. ) );
#9581 = EDGE_LOOP ( 'NONE', ( #14345, #3656, #4165, #10022 ) ) ;
#9582 = EDGE_LOOP ( 'NONE', ( #14856, #14789, #1095, #1718 ) ) ;
#9583 = AXIS2_PLACEMENT_3D ( 'NONE', #8626, #9625, #8548 ) ;
#9584 = VECTOR ( 'NONE', #5866, 1000.000000000000114 ) ;
#9585 = CARTESIAN_POINT ( 'NONE',  ( 5.263246529796798079, -37.53054613522389360, 50.73053146564911486 ) ) ;
#9586 = ORIENTED_EDGE ( 'NONE', *, *, #849, .T. ) ;
#9587 = CARTESIAN_POINT ( 'NONE',  ( 13.85920135429429934, -27.00737899243800300, 43.21206422150100224 ) ) ;
#9588 = CARTESIAN_POINT ( 'NONE',  ( -10.95221305062249506, -4.629260458021023261, 54.00231026484399166 ) ) ;
#9589 = CARTESIAN_POINT ( 'NONE',  ( -7.768926039458054156, -39.58069824233449907, -10.42437048525951404 ) ) ;
#9590 = DIRECTION ( 'NONE',  ( 8.018662683283438208E-16, -5.975035461963189015E-16, -1.000000000000000000 ) ) ;
#9591 = AXIS2_PLACEMENT_3D ( 'NONE', #7163, #2670, #2442 ) ;
#9592 = VECTOR ( 'NONE', #14400, 1000.000000000000000 ) ;
#9593 = CARTESIAN_POINT ( 'NONE',  ( -23.54290256004220439, -7.607589560680598773, 57.00231026484397745 ) ) ;
#9594 = EDGE_CURVE ( 'NONE', #12480, #9329, #4607, .T. ) ;
#9596 = FACE_BOUND ( 'NONE', #148, .T. ) ;
#9595 = CARTESIAN_POINT ( 'NONE',  ( -32.76014075162859740, 10.68321993080349763, 16.26994987741149856 ) ) ;
#9597 = EDGE_LOOP ( 'NONE', ( #11026, #3480, #3754, #3846 ) ) ;
#9598 = FACE_OUTER_BOUND ( 'NONE', #5456, .T. ) ;
#9599 = CARTESIAN_POINT ( 'NONE',  ( -24.10635587892941345, -18.62637863235598346, 60.71193242789581745 ) ) ;
#9600 = VERTEX_POINT ( 'NONE', #12348 ) ;
#9601 = ORIENTED_EDGE ( 'NONE', *, *, #13012, .F. ) ;
#9602 = CARTESIAN_POINT ( 'NONE',  ( 21.92052230653590428, -29.15398386062915037, 21.76268361306444632 ) ) ;
#9603 = CARTESIAN_POINT ( 'NONE',  ( -21.52375782506408086, -39.21750366204430804, 56.51717219687775184 ) ) ;
#9604 = VERTEX_POINT ( 'NONE', #6220 ) ;
#9605 = CARTESIAN_POINT ( 'NONE',  ( -9.477415257007141491, -39.21568696007443577, -17.51282566149688336 ) ) ;
#9606 = AXIS2_PLACEMENT_3D ( 'NONE', #3371, #6941, #8022 ) ;
#9607 = VECTOR ( 'NONE', #14431, 1000.000000000000000 ) ;
#9608 = PLANE ( 'NONE',  #7548 ) ;
#9609 = LINE ( 'NONE', #6156, #3613 ) ;
#9610 = VECTOR ( 'NONE', #10314, 1000.000000000000114 ) ;
#9611 = PLANE ( 'NONE',  #10398 ) ;
#9612 = EDGE_CURVE ( 'NONE', #1229, #7911, #13575, .T. ) ;
#9613 = DIRECTION ( 'NONE',  ( 0.5975035461963189576, 0.8018662683283437342, 0.000000000000000000 ) ) ;
#9614 = ORIENTED_EDGE ( 'NONE', *, *, #6545, .T. ) ;
#9615 = DIRECTION ( 'NONE',  ( -8.018662683283438208E-16, 5.975035461963189015E-16, 1.000000000000000000 ) ) ;
#9616 = FACE_OUTER_BOUND ( 'NONE', #12836, .T. ) ;
#9617 = ORIENTED_EDGE ( 'NONE', *, *, #2541, .T. ) ;
#9618 = EDGE_CURVE ( 'NONE', #10750, #11940, #4311, .T. ) ;
#9619 = CARTESIAN_POINT ( 'NONE',  ( -7.490307934913750465, -12.48011759562962020, 56.85231026484400019 ) ) ;
#9620 = CARTESIAN_POINT ( 'NONE',  ( -15.49969986081099904, 4.873818854045000037, 24.21206422150099868 ) ) ;
#9621 = ORIENTED_EDGE ( 'NONE', *, *, #11677, .F. ) ;
#9622 = DIRECTION ( 'NONE',  ( -1.000000000000000000, -1.201369187114119994E-15, -9.616040805000176517E-16 ) ) ;
#9623 = VECTOR ( 'NONE', #6361, 1000.000000000000000 ) ;
#9624 = VERTEX_POINT ( 'NONE', #10271 ) ;
#9625 = DIRECTION ( 'NONE',  ( -8.018662683283438208E-16, 5.975035461963189015E-16, 1.000000000000000000 ) ) ;
#9626 = LINE ( 'NONE', #3585, #862 ) ;
#9627 = EDGE_CURVE ( 'NONE', #8100, #9541, #7994, .T. ) ;
#9628 = AXIS2_PLACEMENT_3D ( 'NONE', #27, #12153, #6249 ) ;
#9629 = CARTESIAN_POINT ( 'NONE',  ( -18.30022887753442618, -14.85008914724566509, 57.00231026484397745 ) ) ;
#9630 = DIRECTION ( 'NONE',  ( 0.000000000000000000, -1.000000000000000000, -1.224646799147350002E-16 ) ) ;
#9631 = AXIS2_PLACEMENT_3D ( 'NONE', #11460, #987, #11611 ) ;
#9632 = CARTESIAN_POINT ( 'NONE',  ( -8.744347237509680681, -17.93190845158491342, 56.85231026484400019 ) ) ;
#9633 = EDGE_CURVE ( 'NONE', #2471, #3528, #12731, .T. ) ;
#9634 = ORIENTED_EDGE ( 'NONE', *, *, #8680, .F. ) ;
#9635 = DIRECTION ( 'NONE',  ( -8.018662683283438208E-16, 5.975035461963189015E-16, 1.000000000000000000 ) ) ;
#9636 = EDGE_CURVE ( 'NONE', #5900, #11437, #6736, .T. ) ;
#9637 = CARTESIAN_POINT ( 'NONE',  ( -33.65972808787644510, -40.75169664996035834, 52.31182291862857880 ) ) ;
#9638 = VECTOR ( 'NONE', #12233, 1000.000000000000000 ) ;
#9639 = DIRECTION ( 'NONE',  ( 0.000000000000000000, 1.000000000000000000, 1.224646799147350002E-16 ) ) ;
#9640 = EDGE_CURVE ( 'NONE', #259, #9493, #11992, .T. ) ;
#9641 = ORIENTED_EDGE ( 'NONE', *, *, #8680, .T. ) ;
#9642 = CARTESIAN_POINT ( 'NONE',  ( -22.08930316869620825, -18.17457871440291228, 56.85231026484398598 ) ) ;
#9643 = VERTEX_POINT ( 'NONE', #6889 ) ;
#9645 = ORIENTED_EDGE ( 'NONE', *, *, #2353, .F. ) ;
#9644 = DIRECTION ( 'NONE',  ( 0.000000000000000000, 1.000000000000000000, 0.000000000000000000 ) ) ;
#9646 = VERTEX_POINT ( 'NONE', #6583 ) ;
#9647 = CARTESIAN_POINT ( 'NONE',  ( -5.859109405273538407, -10.94619944609606677, 57.00231026484399166 ) ) ;
#9648 = CARTESIAN_POINT ( 'NONE',  ( -15.47224238247604511, -13.54916519690201149, 56.85231026484398598 ) ) ;
#9649 = VERTEX_POINT ( 'NONE', #3082 ) ;
#9650 = LINE ( 'NONE', #2982, #10877 ) ;
#9651 = B_SPLINE_CURVE_WITH_KNOTS ( 'NONE', 3,
 ( #11094, #6342, #14542, #13254, #5205, #540, #5062, #13400, #12169, #1760, #2765, #7419 ),
 .UNSPECIFIED., .F., .F.,
 ( 4, 2, 2, 2, 2, 4 ),
 ( 0.000000000000000000, 0.2500000000000018319, 0.3750000000000028866, 0.4375000000000027756, 0.5000000000000026645, 1.000000000000000000 ),
 .UNSPECIFIED. ) ;
#9652 = LINE ( 'NONE', #9419, #13458 ) ;
#9653 = CARTESIAN_POINT ( 'NONE',  ( -17.49501007863569768, -9.463173585252677711, -13.23580647107073638 ) ) ;
#9654 = ADVANCED_FACE ( 'NONE', ( #11421 ), #797, .F. ) ;
#9655 = CARTESIAN_POINT ( 'NONE',  ( -20.61203582816999713, -107.1622034095870077, -6.087689735156005533 ) ) ;
#9656 = PLANE ( 'NONE',  #2970 ) ;
#9657 = ORIENTED_EDGE ( 'NONE', *, *, #6459, .T. ) ;
#9658 = CARTESIAN_POINT ( 'NONE',  ( -27.49969986081100259, -57.00737899243800655, 55.03046811182510112 ) ) ;
#9659 = VERTEX_POINT ( 'NONE', #871 ) ;
#9660 = ORIENTED_EDGE ( 'NONE', *, *, #9052, .T. ) ;
#9661 = LINE ( 'NONE', #5222, #5410 ) ;
#9662 = ORIENTED_EDGE ( 'NONE', *, *, #16, .F. ) ;
#9663 = ORIENTED_EDGE ( 'NONE', *, *, #14355, .T. ) ;
#9664 = DIRECTION ( 'NONE',  ( -8.018662683283438208E-16, 5.975035461963189015E-16, 1.000000000000000000 ) ) ;
#9665 = PRODUCT_DEFINITION_SHAPE ( 'NONE', 'NONE',  #4799 ) ;
#9666 = DIRECTION ( 'NONE',  ( 0.5975035461963189576, 0.8018662683283437342, 0.000000000000000000 ) ) ;
#9667 = EDGE_CURVE ( 'NONE', #6551, #12278, #10162, .T. ) ;
#9668 = PLANE ( 'NONE',  #7325 ) ;
#9669 = CARTESIAN_POINT ( 'NONE',  ( -22.04595456446742929, -18.23578246029658345, 57.00231026484397745 ) ) ;
#9670 = VECTOR ( 'NONE', #13976, 1000.000000000000000 ) ;
#9671 = PLANE ( 'NONE',  #11345 ) ;
#9673 = CARTESIAN_POINT ( 'NONE',  ( -37.91969009334108165, 5.009117329194947565, 20.24816411459976706 ) ) ;
#9672 = CARTESIAN_POINT ( 'NONE',  ( -13.18491133144367389, -15.23222315862922827, 51.25231026484399166 ) ) ;
#9674 = ORIENTED_EDGE ( 'NONE', *, *, #8404, .F. ) ;
#9675 = DIRECTION ( 'NONE',  ( -0.3956847857120158740, 0.9183863840214728791, 0.000000000000000000 ) ) ;
#9676 = CARTESIAN_POINT ( 'NONE',  ( -19.87664613915258371, -5.557310358991672139, 56.85231026484398598 ) ) ;
#9677 = VERTEX_POINT ( 'NONE', #1018 ) ;
#9678 = ORIENTED_EDGE ( 'NONE', *, *, #4536, .F. ) ;
#9679 = DIRECTION ( 'NONE',  ( 0.000000000000000000, -1.000000000000000000, -1.224646799147350002E-16 ) ) ;
#9680 = CARTESIAN_POINT ( 'NONE',  ( -37.04494295528539993, 12.99262100756199878, 32.26206422150099939 ) ) ;
#9681 = ORIENTED_EDGE ( 'NONE', *, *, #15052, .T. ) ;
#9682 = DIRECTION ( 'NONE',  ( 1.000000000000000000, 0.000000000000000000, 0.000000000000000000 ) ) ;
#9683 = VECTOR ( 'NONE', #5283, 1000.000000000000000 ) ;
#9684 = EDGE_CURVE ( 'NONE', #14495, #13725, #5677, .T. ) ;
#9685 = CARTESIAN_POINT ( 'NONE',  ( 7.200737182676100190, 4.873818854045000037, 27.91208557747711083 ) ) ;
#9686 = CARTESIAN_POINT ( 'NONE',  ( -10.99662508417897477, -22.43611682583629019, 56.73095874158131124 ) ) ;
#9687 = FACE_OUTER_BOUND ( 'NONE', #12583, .T. ) ;
#9688 = CARTESIAN_POINT ( 'NONE',  ( -15.49969986081099194, -27.00737899243800300, 19.50231026484399877 ) ) ;
#9689 = ORIENTED_EDGE ( 'NONE', *, *, #8776, .T. ) ;
#9690 = CARTESIAN_POINT ( 'NONE',  ( -21.05979293892203330, -6.334749421441233430, 56.85231026484398598 ) ) ;
#9691 = AXIS2_PLACEMENT_3D ( 'NONE', #5280, #12323, #9940 ) ;
#9692 = CARTESIAN_POINT ( 'NONE',  ( -7.512805849530849400, -44.04964101872660365, -5.039951761444699585 ) ) ;
#9693 = EDGE_LOOP ( 'NONE', ( #11262, #1422, #9950, #5992, #12057 ) ) ;
#9694 = DIRECTION ( 'NONE',  ( 0.000000000000000000, 1.000000000000000000, 1.224646799147350002E-16 ) ) ;
#9695 = CARTESIAN_POINT ( 'NONE',  ( -15.42469986081099442, -23.50709773848280904, 54.00231026484400587 ) ) ;
#9696 = ORIENTED_EDGE ( 'NONE', *, *, #13256, .F. ) ;
#9697 = ORIENTED_EDGE ( 'NONE', *, *, #8888, .T. ) ;
#9698 = VECTOR ( 'NONE', #6720, 1000.000000000000000 ) ;
#9699 = DIRECTION ( 'NONE',  ( 0.000000000000000000, 0.000000000000000000, 1.000000000000000000 ) ) ;
#9700 = PRODUCT_DEFINITION_SHAPE ( 'NONE', 'NONE',  #15136 ) ;
#9701 = EDGE_CURVE ( 'NONE', #12465, #13214, #4360, .T. ) ;
#9702 = CARTESIAN_POINT ( 'NONE',  ( 4.000300139189000959, -20.37340439622241917, -12.52892449124999885 ) ) ;
#9703 = CIRCLE ( 'NONE', #3837, 0.2000000000000012046 ) ;
#9704 = EDGE_CURVE ( 'NONE', #13117, #2290, #9578, .T. ) ;
#9705 = DIRECTION ( 'NONE',  ( -8.018662683283438208E-16, 5.975035461963189015E-16, 1.000000000000000000 ) ) ;
#9706 = MECHANICAL_DESIGN_GEOMETRIC_PRESENTATION_REPRESENTATION (  '', ( #666 ), #10187 ) ;
#9707 = DIRECTION ( 'NONE',  ( -1.000000000000000000, 0.000000000000000000, 0.000000000000000000 ) ) ;
#9708 = CARTESIAN_POINT ( 'NONE',  ( -15.49969986081091555, -110.0073789924380065, -5.497689735156000346 ) ) ;
#9709 = VERTEX_POINT ( 'NONE', #2618 ) ;
#9710 = CARTESIAN_POINT ( 'NONE',  ( -7.499699860810999041, -44.50737899243799944, -109.5506571639849938 ) ) ;
#9711 = CARTESIAN_POINT ( 'NONE',  ( -38.20013690429809827, 4.873818854045000037, 20.51204286552489009 ) ) ;
#9712 = ORIENTED_EDGE ( 'NONE', *, *, #11118, .F. ) ;
#9713 = CARTESIAN_POINT ( 'NONE',  ( -7.504568435050878783, -44.41879534613468650, -4.116207154834379267 ) ) ;
#9714 = ORIENTED_EDGE ( 'NONE', *, *, #8945, .F. ) ;
#9715 = AXIS2_PLACEMENT_3D ( 'NONE', #14735, #4032, #736 ) ;
#9717 = VERTEX_POINT ( 'NONE', #14254 ) ;
#9716 = CARTESIAN_POINT ( 'NONE',  ( -33.55125091640665147, -41.28719780951828966, -13.36700348819730699 ) ) ;
#9718 = VERTEX_POINT ( 'NONE', #11721 ) ;
#9719 = CIRCLE ( 'NONE', #3853, 9.974999999999999645 ) ;
#9720 = CARTESIAN_POINT ( 'NONE',  ( -1.508527451664999575, -47.37340439622244048, -6.997689735156000346 ) ) ;
#9721 = DIRECTION ( 'NONE',  ( -8.018662683283438208E-16, 5.975035461963189015E-16, 1.000000000000000000 ) ) ;
#9722 = ADVANCED_FACE ( 'NONE', ( #5897 ), #30, .T. ) ;
#9723 = EDGE_CURVE ( 'NONE', #14455, #10539, #1615, .T. ) ;
#9724 = CARTESIAN_POINT ( 'NONE',  ( -17.61203582817000068, -107.1622034095870077, -6.087689735156001980 ) ) ;
#9725 = EDGE_CURVE ( 'NONE', #10291, #5981, #10730, .T. ) ;
#9726 = DIRECTION ( 'NONE',  ( 0.9183863840214729901, 0.3956847857120157075, 4.999999999999999402E-16 ) ) ;
#9727 = APPLICATION_PROTOCOL_DEFINITION ( 'draft international standard', 'automotive_design', 1998, #2935 ) ;
#9728 = CIRCLE ( 'NONE', #14115, 2.999999999999999112 ) ;
#9729 = CARTESIAN_POINT ( 'NONE',  ( -27.49969986081100259, -57.00737899243800655, -16.02584758213710003 ) ) ;
#9730 = AXIS2_PLACEMENT_3D ( 'NONE', #11173, #1689, #13334 ) ;
#9731 = EDGE_CURVE ( 'NONE', #14388, #6962, #3917, .T. ) ;
#9732 = DIRECTION ( 'NONE',  ( 0.000000000000000000, -1.131341397376178819E-16, 1.000000000000000000 ) ) ;
#9733 = VERTEX_POINT ( 'NONE', #2695 ) ;
#9734 = CARTESIAN_POINT ( 'NONE',  ( -8.703838785437527648, -17.86878899887247130, 56.85231026484400019 ) ) ;
#9735 = ORIENTED_EDGE ( 'NONE', *, *, #14769, .F. ) ;
#9736 = DIRECTION ( 'NONE',  ( 0.000000000000000000, 1.272130549049658454E-16, -1.000000000000000000 ) ) ;
#9737 = ORIENTED_EDGE ( 'NONE', *, *, #14574, .T. ) ;
#9738 = VERTEX_POINT ( 'NONE', #5214 ) ;
#9739 = DIRECTION ( 'NONE',  ( -8.018662683283438208E-16, 5.975035461963189015E-16, 1.000000000000000000 ) ) ;
#9740 = ORIENTED_EDGE ( 'NONE', *, *, #7464, .F. ) ;
#9741 = DIRECTION ( 'NONE',  ( -8.018662683283438208E-16, 5.975035461963189015E-16, 1.000000000000000000 ) ) ;
#9742 = VECTOR ( 'NONE', #10666, 1000.000000000000000 ) ;
#9743 = EDGE_CURVE ( 'NONE', #2536, #13533, #8575, .T. ) ;
#9744 = FACE_OUTER_BOUND ( 'NONE', #12584, .T. ) ;
#9745 = DIRECTION ( 'NONE',  ( 8.018662683283438208E-16, -5.975035461963189015E-16, -1.000000000000000000 ) ) ;
#9746 = VECTOR ( 'NONE', #4075, 1000.000000000000000 ) ;
#9747 = LINE ( 'NONE', #3706, #2798 ) ;
#9749 = PLANE ( 'NONE',  #12570 ) ;
#9748 = CARTESIAN_POINT ( 'NONE',  ( -7.505482346041832287, -44.32791517324671560, 20.74177506415496453 ) ) ;
#9750 = ORIENTED_EDGE ( 'NONE', *, *, #4800, .T. ) ;
#9751 = DIRECTION ( 'NONE',  ( 0.5975035461963189576, 0.8018662683283437342, 0.000000000000000000 ) ) ;
#9752 = ORIENTED_EDGE ( 'NONE', *, *, #590, .T. ) ;
#9753 = FACE_OUTER_BOUND ( 'NONE', #1534, .T. ) ;
#9754 = EDGE_LOOP ( 'NONE', ( #6497, #9811, #9504, #8484, #2902 ) ) ;
#9755 = ORIENTED_EDGE ( 'NONE', *, *, #8868, .F. ) ;
#9756 = CARTESIAN_POINT ( 'NONE',  ( 21.86810610412018718, -27.84960833679321368, 21.06582514182977306 ) ) ;
#9757 = EDGE_CURVE ( 'NONE', #4806, #6735, #5070, .T. ) ;
#9758 = CARTESIAN_POINT ( 'NONE',  ( -14.76203582816999926, -107.4618831711941169, -7.659374194735305785 ) ) ;
#9759 = ORIENTED_EDGE ( 'NONE', *, *, #8888, .F. ) ;
#9760 = AXIS2_PLACEMENT_3D ( 'NONE', #9158, #11612, #11462 ) ;
#9761 = AXIS2_PLACEMENT_3D ( 'NONE', #12458, #6617, #6195 ) ;
#9762 = CARTESIAN_POINT ( 'NONE',  ( -15.49969986081099904, 70.81438635534659909, 24.21206422150100579 ) ) ;
#9763 = CARTESIAN_POINT ( 'NONE',  ( -15.49969986081092088, -13.50737899243822504, 56.85231026484398598 ) ) ;
#9764 = AXIS2_PLACEMENT_3D ( 'NONE', #1895, #1665, #6321 ) ;
#9765 = CARTESIAN_POINT ( 'NONE',  ( -15.49969986081099904, 64.39262100756199914, 24.21206422150100579 ) ) ;
#9766 = CYLINDRICAL_SURFACE ( 'NONE', #6178, 8.000000000000000000 ) ;
#9767 = EDGE_LOOP ( 'NONE', ( #4787, #15094, #10039, #615 ) ) ;
#9768 = CARTESIAN_POINT ( 'NONE',  ( -7.506093261461533217, -14.65346081099998088, 56.85231026484400019 ) ) ;
#9769 = CARTESIAN_POINT ( 'NONE',  ( -31.79969986081099975, 11.99262100756199878, 24.16206422150099797 ) ) ;
#9770 = ORIENTED_EDGE ( 'NONE', *, *, #14236, .T. ) ;
#9771 = ADVANCED_FACE ( 'NONE', ( #4998 ), #13481, .F. ) ;
#9772 =( REPRESENTATION_RELATIONSHIP ('NONE','NONE', #2372, #3931 ) REPRESENTATION_RELATIONSHIP_WITH_TRANSFORMATION ( #6918 )SHAPE_REPRESENTATION_RELATIONSHIP( ) );
#9773 = FACE_OUTER_BOUND ( 'NONE', #8373, .T. ) ;
#9774 = CARTESIAN_POINT ( 'NONE',  ( 4.500300139189000959, -19.50737899243801010, 55.93350807262470425 ) ) ;
#9775 = ORIENTED_EDGE ( 'NONE', *, *, #11730, .F. ) ;
#9776 = DIRECTION ( 'NONE',  ( -1.000000000000000000, 1.291538348938060198E-32, -1.054621095516909827E-16 ) ) ;
#9777 = ORIENTED_EDGE ( 'NONE', *, *, #6627, .T. ) ;
#9778 = DIRECTION ( 'NONE',  ( -1.000000000000000000, -1.156482317317871331E-15, -1.011922027653137537E-15 ) ) ;
#9779 = B_SPLINE_CURVE_WITH_KNOTS ( 'NONE', 3,
 ( #5638, #8002, #13909, #12773, #4502, #6853, #2434, #2285, #9462, #3502, #14136, #3658, #3577, #6996, #12617, #6925, #2128, #986, #1126 ),
 .UNSPECIFIED., .F., .F.,
 ( 4, 2, 2, 2, 1, 1, 1, 1, 1, 2, 2, 4 ),
 ( 0.000000000000000000, 0.2500000000003188005, 0.3750000000004767853, 0.4375000000005559442, 0.4687500000005985212, 0.4843750000006151191, 0.4921875000006234457, 0.4960937500006278311, 0.4980468750006310508, 0.4990234375006316614, 0.5000000000006321610, 1.000000000000000000 ),
 .UNSPECIFIED. ) ;
#9780 = FACE_OUTER_BOUND ( 'NONE', #7959, .T. ) ;
#9781 = DIRECTION ( 'NONE',  ( 0.000000000000000000, 0.000000000000000000, -1.000000000000000000 ) ) ;
#9782 = AXIS2_PLACEMENT_3D ( 'NONE', #6212, #1858, #14412 ) ;
#9783 = CARTESIAN_POINT ( 'NONE',  ( 15.21195308717482497, -29.07207680555242035, 2.693057569154425845 ) ) ;
#9784 = DIRECTION ( 'NONE',  ( 0.5975035461963189576, 0.8018662683283437342, 0.000000000000000000 ) ) ;
#9785 = ORIENTED_EDGE ( 'NONE', *, *, #5602, .F. ) ;
#9786 = PLANE ( 'NONE',  #10430 ) ;
#9787 = DIRECTION ( 'NONE',  ( -0.9645173894937585368, -0.2640193276336892936, -6.156614753256587028E-16 ) ) ;
#9788 = ADVANCED_FACE ( 'NONE', ( #2841 ), #9656, .F. ) ;
#9789 = EDGE_LOOP ( 'NONE', ( #13645, #1800, #6984, #2697 ) ) ;
#9790 = CARTESIAN_POINT ( 'NONE',  ( -24.33650094517379614, -11.44044972528773130, 56.85231026484398598 ) ) ;
#9791 = ORIENTED_EDGE ( 'NONE', *, *, #9892, .F. ) ;
#9793 = ORIENTED_EDGE ( 'NONE', *, *, #13170, .F. ) ;
#9792 = FACE_OUTER_BOUND ( 'NONE', #9311, .T. ) ;
#9794 = VERTEX_POINT ( 'NONE', #12255 ) ;
#9795 = DIRECTION ( 'NONE',  ( 0.000000000000000000, 0.000000000000000000, 1.000000000000000000 ) ) ;
#9796 = ORIENTED_EDGE ( 'NONE', *, *, #4626, .T. ) ;
#9797 = LINE ( 'NONE', #14462, #7189 ) ;
#9798 = LINE ( 'NONE', #12170, #6263 ) ;
#9799 = DIRECTION ( 'NONE',  ( 0.4224988092984258703, 0.5670050759397237128, 0.7071067811865479058 ) ) ;
#9800 = AXIS2_PLACEMENT_3D ( 'NONE', #4185, #9144, #12301 ) ;
#9801 = CARTESIAN_POINT ( 'NONE',  ( -7.510314868261046328, -44.09321551920025684, 45.16549881609444128 ) ) ;
#9802 = EDGE_CURVE ( 'NONE', #2549, #3663, #9812, .T. ) ;
#9803 = VERTEX_POINT ( 'NONE', #1848 ) ;
#9804 = LINE ( 'NONE', #11023, #2247 ) ;
#9805 = ORIENTED_EDGE ( 'NONE', *, *, #2763, .F. ) ;
#9806 = CARTESIAN_POINT ( 'NONE',  ( 2.500300139188999182, -51.00737899243799944, 52.39987856403599409 ) ) ;
#9807 = ORIENTED_EDGE ( 'NONE', *, *, #1414, .T. ) ;
#9808 = ORIENTED_EDGE ( 'NONE', *, *, #9636, .F. ) ;
#9809 = EDGE_CURVE ( 'NONE', #5736, #9278, #1695, .T. ) ;
#9810 = CARTESIAN_POINT ( 'NONE',  ( -3.508527451665000463, -45.64135358865355840, -6.997689735156000346 ) ) ;
#9811 = ORIENTED_EDGE ( 'NONE', *, *, #5048, .T. ) ;
#9812 = CIRCLE ( 'NONE', #10047, 9.974999999999999645 ) ;
#9813 = CARTESIAN_POINT ( 'NONE',  ( -17.73437360760467030, -13.24520873212868644, 51.00231026484399166 ) ) ;
#9814 = EDGE_CURVE ( 'NONE', #8623, #6681, #2992, .T. ) ;
#9815 = DIRECTION ( 'NONE',  ( 0.5975035461963189576, 0.8018662683283437342, 0.000000000000000000 ) ) ;
#9816 = LINE ( 'NONE', #7590, #11694 ) ;
#9817 = AXIS2_PLACEMENT_3D ( 'NONE', #345, #8730, #4150 ) ;
#9818 = EDGE_CURVE ( 'NONE', #12839, #2212, #1518, .T. ) ;
#9819 = AXIS2_PLACEMENT_3D ( 'NONE', #11561, #9030, #8337 ) ;
#9820 = AXIS2_PLACEMENT_3D ( 'NONE', #13445, #8829, #12291 ) ;
#9822 = LINE ( 'NONE', #12051, #4743 ) ;
#9821 = LINE ( 'NONE', #3079, #8327 ) ;
#9823 = EDGE_CURVE ( 'NONE', #7809, #1380, #6201, .T. ) ;
#9824 = ORIENTED_EDGE ( 'NONE', *, *, #7170, .T. ) ;
#9825 = DIRECTION ( 'NONE',  ( -0.9868311969055005850, -0.1617534816134010012, -6.946583704589984503E-16 ) ) ;
#9826 = EDGE_CURVE ( 'NONE', #9434, #7024, #8589, .T. ) ;
#9827 = DIRECTION ( 'NONE',  ( -1.000000000000000000, 0.000000000000000000, 0.000000000000000000 ) ) ;
#9828 = EDGE_LOOP ( 'NONE', ( #4391, #14161, #10027, #14441 ) ) ;
#9829 = ORIENTED_EDGE ( 'NONE', *, *, #9921, .F. ) ;
#9830 = CARTESIAN_POINT ( 'NONE',  ( -22.44301654231075815, -48.51543857339960653, 56.35509430644546569 ) ) ;
#9831 = EDGE_LOOP ( 'NONE', ( #5379, #10130, #7486, #4319 ) ) ;
#9832 = DIRECTION ( 'NONE',  ( -8.018662683283438208E-16, 5.975035461963189015E-16, 1.000000000000000000 ) ) ;
#9833 = VECTOR ( 'NONE', #11668, 1000.000000000000000 ) ;
#9834 = AXIS2_PLACEMENT_3D ( 'NONE', #11388, #11243, #5568 ) ;
#9835 = CIRCLE ( 'NONE', #9819, 1.300000000000000488 ) ;
#9836 = VECTOR ( 'NONE', #10857, 1000.000000000000114 ) ;
#9837 = CARTESIAN_POINT ( 'NONE',  ( 6.638443592182626141, 5.145091203767020005, 19.98296810155703085 ) ) ;
#9838 = CARTESIAN_POINT ( 'NONE',  ( -20.60655739512266749, -107.0640443292477073, -7.162689735156005710 ) ) ;
#9839 = CARTESIAN_POINT ( 'NONE',  ( -11.06590827715117520, -22.47078556645032066, 56.73927296486425575 ) ) ;
#9840 = CARTESIAN_POINT ( 'NONE',  ( -23.49969986081100615, -39.82108749142274462, 14.81601876382873506 ) ) ;
#9841 = CARTESIAN_POINT ( 'NONE',  ( -15.49969986081086226, -13.50737899243826767, -13.49768973515600301 ) ) ;
#9842 = ORIENTED_EDGE ( 'NONE', *, *, #4215, .T. ) ;
#9843 = CARTESIAN_POINT ( 'NONE',  ( -21.45979773411920277, -21.50599501901345434, 54.00231026484399166 ) ) ;
#9844 = EDGE_CURVE ( 'NONE', #1516, #9043, #6349, .T. ) ;
#9845 = CARTESIAN_POINT ( 'NONE',  ( -15.49969986081099194, -110.2236589786222538, -11.14993866902398700 ) ) ;
#9846 = EDGE_LOOP ( 'NONE', ( #9955, #3923, #12451, #7704 ) ) ;
#9847 = EDGE_CURVE ( 'NONE', #14164, #12982, #9804, .T. ) ;
#9848 = CARTESIAN_POINT ( 'NONE',  ( 21.86810272172535363, -26.16575740022191709, 27.35833972362090094 ) ) ;
#9849 =( LENGTH_UNIT ( ) NAMED_UNIT ( * ) SI_UNIT ( .MILLI., .METRE. ) );
#9850 = EDGE_LOOP ( 'NONE', ( #12389, #3826, #319, #2274 ) ) ;
#9851 = CARTESIAN_POINT ( 'NONE',  ( -23.49969986081099904, -44.50737899243799944, -109.5506571639849938 ) ) ;
#9852 = ORIENTED_EDGE ( 'NONE', *, *, #9474, .F. ) ;
#9853 = DIRECTION ( 'NONE',  ( -0.9472588896649086765, 0.3204693369899911382, -9.510565162951535624E-16 ) ) ;
#9854 = VECTOR ( 'NONE', #12981, 1000.000000000000227 ) ;
#9855 = EDGE_CURVE ( 'NONE', #9045, #6888, #4144, .T. ) ;
#9856 = AXIS2_PLACEMENT_3D ( 'NONE', #8257, #4984, #12950 ) ;
#9857 = CARTESIAN_POINT ( 'NONE',  ( -7.886584594865190034, -46.96511696614940234, 17.04457229113261718 ) ) ;
#9858 = AXIS2_PLACEMENT_3D ( 'NONE', #5251, #734, #2031 ) ;
#9859 = DIRECTION ( 'NONE',  ( -0.1511109077013120527, -0.9885168150181793401, 4.694715627858928842E-16 ) ) ;
#9860 = CARTESIAN_POINT ( 'NONE',  ( 0.8003001391889992266, 20.99262100756200056, 32.26206422150099939 ) ) ;
#9861 = ORIENTED_EDGE ( 'NONE', *, *, #6443, .F. ) ;
#9862 = DIRECTION ( 'NONE',  ( -8.018662683283438208E-16, 5.975035461963189015E-16, 1.000000000000000000 ) ) ;
#9863 = CARTESIAN_POINT ( 'NONE',  ( -24.88854884048805971, -16.87637585156647191, 56.85231026484398598 ) ) ;
#9864 = ORIENTED_EDGE ( 'NONE', *, *, #4683, .T. ) ;
#9865 = ORIENTED_EDGE ( 'NONE', *, *, #14466, .T. ) ;
#9867 = ORIENTED_EDGE ( 'NONE', *, *, #1201, .F. ) ;
#9866 = CARTESIAN_POINT ( 'NONE',  ( -36.05468215437335289, -37.64246294775075796, -11.86277418255565053 ) ) ;
#9868 = ORIENTED_EDGE ( 'NONE', *, *, #2780, .T. ) ;
#9869 = VECTOR ( 'NONE', #2043, 1000.000000000000000 ) ;
#9870 = DIRECTION ( 'NONE',  ( -8.018662683283439195E-16, 5.975035461963190001E-16, 1.000000000000000000 ) ) ;
#9871 = ORIENTED_EDGE ( 'NONE', *, *, #14953, .T. ) ;
#9872 = CARTESIAN_POINT ( 'NONE',  ( -20.45368390747784204, -7.130130991507916072, 56.85231026484398598 ) ) ;
#9873 = LINE ( 'NONE', #475, #9893 ) ;
#9874 = AXIS2_PLACEMENT_3D ( 'NONE', #510, #12212, #6377 ) ;
#9875 = EDGE_CURVE ( 'NONE', #6512, #6717, #4065, .T. ) ;
#9876 = DIRECTION ( 'NONE',  ( -1.000000000000000000, -1.201369187114119994E-15, -9.616040805000176517E-16 ) ) ;
#9877 = LINE ( 'NONE', #6271, #14376 ) ;
#9878 = VECTOR ( 'NONE', #8193, 1000.000000000000000 ) ;
#9879 = DIRECTION ( 'NONE',  ( -0.9183863840214729901, -0.3956847857120157075, -4.999999999999999402E-16 ) ) ;
#9880 = DIRECTION ( 'NONE',  ( -0.2536112499260171349, -0.9673062255102895524, 3.746065934159117949E-16 ) ) ;
#9881 = VERTEX_POINT ( 'NONE', #2921 ) ;
#9882 = CARTESIAN_POINT ( 'NONE',  ( 0.5796456139481083181, -52.92803351767888387, 53.45077026338344695 ) ) ;
#9884 = ORIENTED_EDGE ( 'NONE', *, *, #7855, .F. ) ;
#9883 = LINE ( 'NONE', #4293, #12060 ) ;
#9885 = ORIENTED_EDGE ( 'NONE', *, *, #2920, .T. ) ;
#9886 = CARTESIAN_POINT ( 'NONE',  ( -15.45378054160984682, -13.48759475315262613, 56.85231026484398598 ) ) ;
#9887 = ORIENTED_EDGE ( 'NONE', *, *, #3746, .T. ) ;
#9888 = LINE ( 'NONE', #2779, #2916 ) ;
#9889 = EDGE_CURVE ( 'NONE', #12295, #15022, #2004, .T. ) ;
#9890 = CARTESIAN_POINT ( 'NONE',  ( -14.95642007119156425, -3.547184613301258782, 56.85231026484398598 ) ) ;
#9891 = CARTESIAN_POINT ( 'NONE',  ( 9.000300139189000959, -27.00737899243800300, 7.712064221501001349 ) ) ;
#9892 = EDGE_CURVE ( 'NONE', #13194, #12587, #7646, .T. ) ;
#9893 = VECTOR ( 'NONE', #14394, 1000.000000000000227 ) ;
#9895 = CARTESIAN_POINT ( 'NONE',  ( -35.79506410546698447, 6.030134292668329898, 18.82790939717704504 ) ) ;
#9894 = FACE_OUTER_BOUND ( 'NONE', #2649, .T. ) ;
#9896 = ORIENTED_EDGE ( 'NONE', *, *, #9346, .F. ) ;
#9897 = CARTESIAN_POINT ( 'NONE',  ( -15.49969986081099904, 2.992621007561999669, 1.212064221501000461 ) ) ;
#9898 = ORIENTED_EDGE ( 'NONE', *, *, #5870, .F. ) ;
#9899 = CARTESIAN_POINT ( 'NONE',  ( -15.47224238247604511, -13.54916519690201149, 56.85231026484398598 ) ) ;
#9900 = EDGE_LOOP ( 'NONE', ( #1791, #2174 ) ) ;
#9901 = EDGE_LOOP ( 'NONE', ( #12803, #4374, #9011, #3260 ) ) ;
#9902 = CARTESIAN_POINT ( 'NONE',  ( 22.00030013918900096, -27.00737899243800300, 26.71206422150099868 ) ) ;
#9903 = VERTEX_POINT ( 'NONE', #8876 ) ;
#9904 = DIRECTION ( 'NONE',  ( -1.000000000000000000, 0.000000000000000000, 0.000000000000000000 ) ) ;
#9905 = ADVANCED_FACE ( 'NONE', ( #6492 ), #6645, .T. ) ;
#9906 = LINE ( 'NONE', #8398, #1590 ) ;
#9907 = CARTESIAN_POINT ( 'NONE',  ( -16.73644428586259636, -23.40541355628490550, 56.85231026484400019 ) ) ;
#9908 = EDGE_CURVE ( 'NONE', #7829, #12833, #6570, .T. ) ;
#9909 = DIRECTION ( 'NONE',  ( 0.000000000000000000, 1.850371707708594316E-16, -1.000000000000000000 ) ) ;
#9910 = DIRECTION ( 'NONE',  ( -8.018662683283438208E-16, 5.975035461963189015E-16, 1.000000000000000000 ) ) ;
#9911 = DIRECTION ( 'NONE',  ( 8.018662683283438208E-16, -5.975035461963189015E-16, -1.000000000000000000 ) ) ;
#9912 = ORIENTED_EDGE ( 'NONE', *, *, #11245, .F. ) ;
#9913 = CARTESIAN_POINT ( 'NONE',  ( -12.93661424846659358, -15.26135318755250658, 57.00231026484399166 ) ) ;
#9914 = PLANE ( 'NONE',  #1674 ) ;
#9915 = EDGE_LOOP ( 'NONE', ( #3980, #11996, #3696, #3901 ) ) ;
#9916 = EDGE_CURVE ( 'NONE', #14313, #259, #7836, .T. ) ;
#9917 = AXIS2_PLACEMENT_3D ( 'NONE', #6399, #7551, #13680 ) ;
#9918 = DIRECTION ( 'NONE',  ( -0.9354976265738682573, 0.3533329742249642913, -9.612616959383187437E-16 ) ) ;
#9919 = VERTEX_POINT ( 'NONE', #11329 ) ;
#9920 = CARTESIAN_POINT ( 'NONE',  ( -3.508527451665000463, -45.20834088676133433, -6.247689735156000346 ) ) ;
#9921 = EDGE_CURVE ( 'NONE', #5844, #8821, #13702, .T. ) ;
#9922 = CARTESIAN_POINT ( 'NONE',  ( -7.799975386333939831, -47.73689692355232239, 17.32552578446427560 ) ) ;
#9923 = EDGE_CURVE ( 'NONE', #2754, #1528, #8947, .T. ) ;
#9924 = DIRECTION ( 'NONE',  ( 0.000000000000000000, 0.000000000000000000, 1.000000000000000000 ) ) ;
#9925 = CARTESIAN_POINT ( 'NONE',  ( 0.1306401100565676154, -27.07585217469822680, -9.967496158821944618 ) ) ;
#9926 = ORIENTED_EDGE ( 'NONE', *, *, #4106, .F. ) ;
#9927 = CARTESIAN_POINT ( 'NONE',  ( -15.04562126104788966, -5.444807279564146896, 56.85231026484398598 ) ) ;
#9928 = CARTESIAN_POINT ( 'NONE',  ( -7.705994742804308295, -46.29709259384130604, -3.005990668410089217 ) ) ;
#9929 = VERTEX_POINT ( 'NONE', #4220 ) ;
#9931 = ORIENTED_EDGE ( 'NONE', *, *, #14886, .F. ) ;
#9930 = DIRECTION ( 'NONE',  ( -0.9316361277244830097, -0.3633925226508256667, -5.299192642332049884E-16 ) ) ;
#9932 = VERTEX_POINT ( 'NONE', #854 ) ;
#9933 = EDGE_CURVE ( 'NONE', #5474, #2549, #699, .T. ) ;
#9934 = CARTESIAN_POINT ( 'NONE',  ( -11.55238169831532957, -21.67927775123549594, 56.85231026484400019 ) ) ;
#9935 = ORIENTED_EDGE ( 'NONE', *, *, #1574, .T. ) ;
#9936 = FACE_OUTER_BOUND ( 'NONE', #8520, .T. ) ;
#9937 = CARTESIAN_POINT ( 'NONE',  ( -21.29301345516119071, -7.881655252552254964, 56.85231026484398598 ) ) ;
#9938 = TOROIDAL_SURFACE ( 'NONE', #8471, 1.600000000000000089, 0.1499999999999999944 ) ;
#9939 = PRODUCT_DEFINITION_SHAPE ( 'NONE', 'NONE',  #15134 ) ;
#9940 = DIRECTION ( 'NONE',  ( 1.508455196501571429E-16, 1.131341397376178572E-16, -1.000000000000000000 ) ) ;
#9941 = LINE ( 'NONE', #13403, #13162 ) ;
#9942 = CARTESIAN_POINT ( 'NONE',  ( -15.49969986081099904, 9.919219809770899232, 24.21206422150099868 ) ) ;
#9943 = VECTOR ( 'NONE', #10002, 1000.000000000000114 ) ;
#9944 = DIRECTION ( 'NONE',  ( -1.291538348938060198E-32, 1.000000000000000000, 0.000000000000000000 ) ) ;
#9945 = AXIS2_PLACEMENT_3D ( 'NONE', #13562, #9109, #3070 ) ;
#9946 = ORIENTED_EDGE ( 'NONE', *, *, #4571, .F. ) ;
#9947 = DIRECTION ( 'NONE',  ( 0.000000000000000000, 0.000000000000000000, 1.000000000000000000 ) ) ;
#9948 = ORIENTED_EDGE ( 'NONE', *, *, #5212, .T. ) ;
#9949 = DIRECTION ( 'NONE',  ( 0.000000000000000000, 0.000000000000000000, -1.000000000000000000 ) ) ;
#9950 = ORIENTED_EDGE ( 'NONE', *, *, #14766, .T. ) ;
#9951 = ORIENTED_EDGE ( 'NONE', *, *, #13293, .T. ) ;
#9952 = EDGE_CURVE ( 'NONE', #8778, #14720, #12560, .T. ) ;
#9953 = PLANE ( 'NONE',  #6875 ) ;
#9955 = ORIENTED_EDGE ( 'NONE', *, *, #8675, .F. ) ;
#9954 = DIRECTION ( 'NONE',  ( -1.000000000000000000, 0.000000000000000000, 0.000000000000000000 ) ) ;
#9956 = LINE ( 'NONE', #9813, #11468 ) ;
#9957 = AXIS2_PLACEMENT_3D ( 'NONE', #3750, #4904, #13389 ) ;
#9958 = CARTESIAN_POINT ( 'NONE',  ( -12.23206416678372932, -4.082773856353237640, 57.00231026484397745 ) ) ;
#9959 = VECTOR ( 'NONE', #10496, 1000.000000000000227 ) ;
#9960 = CARTESIAN_POINT ( 'NONE',  ( -1.508527451665001351, -45.20834088676132723, -6.247689735156000346 ) ) ;
#9961 = APPLICATION_CONTEXT ( 'automotive_design' ) ;
#9963 = LINE ( 'NONE', #13426, #4249 ) ;
#9962 = LINE ( 'NONE', #6511, #6367 ) ;
#9964 = VERTEX_POINT ( 'NONE', #6718 ) ;
#9965 = FACE_OUTER_BOUND ( 'NONE', #9038, .T. ) ;
#9966 = CIRCLE ( 'NONE', #10206, 10.00000000000000000 ) ;
#9967 = ORIENTED_EDGE ( 'NONE', *, *, #10478, .T. ) ;
#9968 = ORIENTED_EDGE ( 'NONE', *, *, #7194, .T. ) ;
#9969 = EDGE_CURVE ( 'NONE', #12278, #6551, #3247, .T. ) ;
#9970 = AXIS2_PLACEMENT_3D ( 'NONE', #6860, #9316, #2429 ) ;
#9971 = FACE_BOUND ( 'NONE', #8659, .T. ) ;
#9972 = ORIENTED_EDGE ( 'NONE', *, *, #7938, .T. ) ;
#9973 = DIRECTION ( 'NONE',  ( 0.000000000000000000, 1.000000000000000000, 1.224646799147350002E-16 ) ) ;
#9974 = EDGE_CURVE ( 'NONE', #8450, #1455, #3374, .T. ) ;
#9975 = VECTOR ( 'NONE', #12046, 1000.000000000000227 ) ;
#9976 = CARTESIAN_POINT ( 'NONE',  ( 4.312229196889595606, 6.261951257096727730, 18.58236366442973519 ) ) ;
#9977 = DIRECTION ( 'NONE',  ( -8.018662683283438208E-16, 5.975035461963189015E-16, 1.000000000000000000 ) ) ;
#9978 = CARTESIAN_POINT ( 'NONE',  ( 14.77511232944436692, -26.09918393201953535, 2.083139152813529904 ) ) ;
#9979 = DIRECTION ( 'NONE',  ( 8.018662683283438208E-16, -5.975035461963189015E-16, -1.000000000000000000 ) ) ;
#9980 = CARTESIAN_POINT ( 'NONE',  ( -1.508527451664999575, -46.50737899243799234, -5.497689735156000346 ) ) ;
#9981 = ORIENTED_EDGE ( 'NONE', *, *, #5208, .T. ) ;
#9982 = CARTESIAN_POINT ( 'NONE',  ( -7.426192534185826588, -13.67980128487994129, 56.85231026484400019 ) ) ;
#9983 = AXIS2_PLACEMENT_3D ( 'NONE', #8802, #6777, #12619 ) ;
#9984 = CARTESIAN_POINT ( 'NONE',  ( -22.54723635769173384, -9.564857042577559199, 57.00231026484397745 ) ) ;
#9985 = EDGE_LOOP ( 'NONE', ( #13631, #2158, #357, #3248 ) ) ;
#9986 = EDGE_CURVE ( 'NONE', #13349, #1855, #4439, .T. ) ;
#9988 = EDGE_CURVE ( 'NONE', #14495, #5451, #13489, .T. ) ;
#9987 = DIRECTION ( 'NONE',  ( -8.018662683283438208E-16, 5.975035461963189015E-16, 1.000000000000000000 ) ) ;
#9989 = DIRECTION ( 'NONE',  ( 0.5975035461963189576, 0.8018662683283437342, 0.000000000000000000 ) ) ;
#9990 = ORIENTED_EDGE ( 'NONE', *, *, #476, .F. ) ;
#9991 = DIRECTION ( 'NONE',  ( 0.000000000000000000, -1.000000000000000000, -1.224646799147350002E-16 ) ) ;
#9992 = VECTOR ( 'NONE', #538, 1000.000000000000000 ) ;
#9993 = ADVANCED_FACE ( 'NONE', ( #8410 ), #8095, .T. ) ;
#9994 = DIRECTION ( 'NONE',  ( -8.018662683283438208E-16, 5.975035461963189015E-16, 1.000000000000000000 ) ) ;
#9995 = AXIS2_PLACEMENT_3D ( 'NONE', #2005, #861, #4453 ) ;
#9996 = EDGE_CURVE ( 'NONE', #13839, #14554, #2380, .T. ) ;
#9997 = CONTEXT_DEPENDENT_SHAPE_REPRESENTATION ( #3226, #2854 ) ;
#9998 = DIRECTION ( 'NONE',  ( 0.000000000000000000, 1.000000000000000000, 1.224646799147350002E-16 ) ) ;
#9999 = LINE ( 'NONE', #13606, #13104 ) ;
#10000 = CARTESIAN_POINT ( 'NONE',  ( -20.19618812003464470, -21.27295997720514720, 57.00231026484397745 ) ) ;
#10001 = ORIENTED_EDGE ( 'NONE', *, *, #9495, .F. ) ;
#10002 = DIRECTION ( 'NONE',  ( 0.9983330752162417054, 0.05771543059946734194, 7.660444431189781397E-16 ) ) ;
#10003 = DIRECTION ( 'NONE',  ( -0.9418150828622243731, -0.3361314470459753623, -9.418150828622246992E-16 ) ) ;
#10004 = ADVANCED_FACE ( 'NONE', ( #2225 ), #9410, .F. ) ;
#10005 = ADVANCED_FACE ( 'NONE', ( #7021 ), #4907, .T. ) ;
#10006 = ORIENTED_EDGE ( 'NONE', *, *, #10952, .T. ) ;
#10008 = ORIENTED_EDGE ( 'NONE', *, *, #5462, .F. ) ;
#10007 = DIRECTION ( 'NONE',  ( -1.000000000000000000, 1.291538348938060198E-32, -1.054621095516909827E-16 ) ) ;
#10009 = VERTEX_POINT ( 'NONE', #6870 ) ;
#10010 = DIRECTION ( 'NONE',  ( 0.7032868978765995926, 0.7109061395677416240, 1.391731009600651544E-16 ) ) ;
#10011 = CARTESIAN_POINT ( 'NONE',  ( -8.209920852191324059, -47.81297650378272834, 56.28708271300973109 ) ) ;
#10012 = LINE ( 'NONE', #9872, #7378 ) ;
#10013 = DIRECTION ( 'NONE',  ( 0.000000000000000000, 1.224646799147350002E-16, -1.000000000000000000 ) ) ;
#10014 = DIRECTION ( 'NONE',  ( 8.018662683283438208E-16, -5.975035461963189015E-16, -1.000000000000000000 ) ) ;
#10015 = EDGE_CURVE ( 'NONE', #5621, #10814, #1429, .T. ) ;
#10016 = CYLINDRICAL_SURFACE ( 'NONE', #14815, 8.000000000000000000 ) ;
#10017 = CARTESIAN_POINT ( 'NONE',  ( -7.512805849530849400, -44.04964101872660365, 19.96004823855532706 ) ) ;
#10018 = DIRECTION ( 'NONE',  ( 0.000000000000000000, 1.000000000000000000, 1.224646799147350002E-16 ) ) ;
#10019 = CARTESIAN_POINT ( 'NONE',  ( 15.03585683394451955, -28.72361223820153242, 45.98022787283635893 ) ) ;
#10020 = VERTEX_POINT ( 'NONE', #4672 ) ;
#10021 = LINE ( 'NONE', #6495, #2179 ) ;
#10022 = ORIENTED_EDGE ( 'NONE', *, *, #9847, .F. ) ;
#10023 = ORIENTED_EDGE ( 'NONE', *, *, #7655, .T. ) ;
#10024 = LINE ( 'NONE', #13415, #3476 ) ;
#10025 = CARTESIAN_POINT ( 'NONE',  ( -15.49969986081092088, -13.50737899243822504, 56.85231026484398598 ) ) ;
#10027 = ORIENTED_EDGE ( 'NONE', *, *, #6198, .T. ) ;
#10026 = CARTESIAN_POINT ( 'NONE',  ( 1.899771560857192121, 9.436645346035778203, 16.57911348776239180 ) ) ;
#10028 = CARTESIAN_POINT ( 'NONE',  ( -14.90935270056153783, -9.036630781709011018, -13.28439369589753483 ) ) ;
#10029 = DIRECTION ( 'NONE',  ( 0.000000000000000000, 9.251858538542971581E-17, -1.000000000000000000 ) ) ;
#10030 = EDGE_CURVE ( 'NONE', #3205, #9069, #14235, .T. ) ;
#10031 = B_SPLINE_CURVE_WITH_KNOTS ( 'NONE', 3,
 ( #691, #12101, #404, #3987, #5065, #14395, #8568, #13257, #10950, #8647, #13333, #8869, #12555, #5574, #14770, #14991, #3212, #7941, #12397, #12629, #13844, #2070, #3364, #11322, #5504, #4438 ),
 .UNSPECIFIED., .F., .F.,
 ( 4, 2, 2, 1, 2, 2, 2, 2, 1, 2, 2, 2, 2, 4 ),
 ( 0.5000307302539015453, 0.5443642001973365563, 0.5665309351690539508, 0.5886976701407714563, 0.6108644051124889618, 0.6330311400842063563, 0.6773646100276413673, 0.6995313449993587618, 0.7216980799710761563, 0.7438648149427934397, 0.7660315499145107232, 0.8103650198579455122, 0.8325317548296629067, 0.8546984898013801901 ),
 .UNSPECIFIED. ) ;
#10032 = EDGE_CURVE ( 'NONE', #11873, #642, #11523, .T. ) ;
#10033 = CARTESIAN_POINT ( 'NONE',  ( 4.000300139189000959, -20.37340439622242982, 51.53354502093799994 ) ) ;
#10034 = CARTESIAN_POINT ( 'NONE',  ( -22.42051587769119791, -8.443926053929422082, 56.85231026484398598 ) ) ;
#10035 = ORIENTED_EDGE ( 'NONE', *, *, #1537, .T. ) ;
#10036 = CARTESIAN_POINT ( 'NONE',  ( -15.49969986081099904, -32.00737899243799944, 24.21206422150099868 ) ) ;
#10037 = FACE_OUTER_BOUND ( 'NONE', #11185, .T. ) ;
#10038 = ORIENTED_EDGE ( 'NONE', *, *, #15052, .F. ) ;
#10039 = ORIENTED_EDGE ( 'NONE', *, *, #9357, .F. ) ;
#10040 = VECTOR ( 'NONE', #4929, 1000.000000000000000 ) ;
#10041 = CARTESIAN_POINT ( 'NONE',  ( 2.500300139188999182, -46.50737899243799944, 19.50231026484399877 ) ) ;
#10042 = ORIENTED_EDGE ( 'NONE', *, *, #9529, .F. ) ;
#10043 = LINE ( 'NONE', #8822, #11056 ) ;
#10044 = CARTESIAN_POINT ( 'NONE',  ( 5.874921005947147279, 5.512834891045747199, 19.41550980370611157 ) ) ;
#10045 = AXIS2_PLACEMENT_3D ( 'NONE', #14874, #4395, #13724 ) ;
#10046 = CARTESIAN_POINT ( 'NONE',  ( 4.806612929222199071, 12.32432269366989530, 32.26206422150099939 ) ) ;
#10047 = AXIS2_PLACEMENT_3D ( 'NONE', #10958, #3840, #12031 ) ;
#10048 = ADVANCED_FACE ( 'NONE', ( #2527 ), #1301, .F. ) ;
#10049 = DIRECTION ( 'NONE',  ( 1.000000000000000000, 1.000000000000000078E-15, 0.000000000000000000 ) ) ;
#10050 = DIRECTION ( 'NONE',  ( -1.000000000000000078E-15, 1.000000000000000000, 0.000000000000000000 ) ) ;
#10052 = CARTESIAN_POINT ( 'NONE',  ( 5.815147591963106599, 5.541088692445907071, 28.99552279544280964 ) ) ;
#10051 = FACE_OUTER_BOUND ( 'NONE', #199, .T. ) ;
#10053 = EDGE_LOOP ( 'NONE', ( #2604, #7366, #7025, #501 ) ) ;
#10054 = CARTESIAN_POINT ( 'NONE',  ( -22.67472226038933059, -17.21206232108429290, 56.85231026484398598 ) ) ;
#10055 = CARTESIAN_POINT ( 'NONE',  ( -31.79969986081099975, 11.99262100756199878, 16.16206422150100153 ) ) ;
#10056 = VERTEX_POINT ( 'NONE', #6027 ) ;
#10057 = CARTESIAN_POINT ( 'NONE',  ( 1.809265100128740311, 10.04760564993946126, 32.04872215841241001 ) ) ;
#10058 = CIRCLE ( 'NONE', #11785, 8.000000000000000000 ) ;
#10059 = DIRECTION ( 'NONE',  ( 1.000000000000000000, -1.291538348938060198E-32, 1.054621095516909827E-16 ) ) ;
#10060 = AXIS2_PLACEMENT_3D ( 'NONE', #14985, #6480, #8083 ) ;
#10061 = CARTESIAN_POINT ( 'NONE',  ( -6.424455519809837867, -13.54187755947681993, 56.85231026484400019 ) ) ;
#10062 = ORIENTED_EDGE ( 'NONE', *, *, #9064, .T. ) ;
#10063 = DIRECTION ( 'NONE',  ( 0.2301973227387160703, -0.9731439732146149879, 7.660444431189776467E-16 ) ) ;
#10064 = VECTOR ( 'NONE', #8601, 1000.000000000000000 ) ;
#10065 = VECTOR ( 'NONE', #7321, 1000.000000000000227 ) ;
#10066 = DIRECTION ( 'NONE',  ( 0.5975035461963188466, 0.8018662683283437342, 0.000000000000000000 ) ) ;
#10067 = EDGE_CURVE ( 'NONE', #572, #4418, #6374, .T. ) ;
#10068 = CARTESIAN_POINT ( 'NONE',  ( -7.570456978157269035, -48.78587553029987589, 20.54355782397079722 ) ) ;
#10069 = VECTOR ( 'NONE', #12971, 1000.000000000000000 ) ;
#10070 = AXIS2_PLACEMENT_3D ( 'NONE', #8502, #5069, #9732 ) ;
#10071 = DIRECTION ( 'NONE',  ( -8.018662683283439195E-16, 5.975035461963190001E-16, 1.000000000000000000 ) ) ;
#10072 = CARTESIAN_POINT ( 'NONE',  ( -15.57469986081099478, -23.50737899243800300, 56.85231026484400019 ) ) ;
#10073 = ADVANCED_FACE ( 'NONE', ( #9487 ), #11701, .T. ) ;
#10074 = ORIENTED_EDGE ( 'NONE', *, *, #9531, .F. ) ;
#10075 = CARTESIAN_POINT ( 'NONE',  ( -15.49969986081099016, -110.5850680553859746, -10.73408862071934067 ) ) ;
#10076 = DIRECTION ( 'NONE',  ( 1.000000000000000000, 1.201369187114119994E-15, 9.616040805000176517E-16 ) ) ;
#10077 = VERTEX_POINT ( 'NONE', #14158 ) ;
#10079 = ORIENTED_EDGE ( 'NONE', *, *, #194, .T. ) ;
#10078 = CARTESIAN_POINT ( 'NONE',  ( -33.70353523260111928, -40.58388572172528086, -13.28296881874997126 ) ) ;
#10080 = ORIENTED_EDGE ( 'NONE', *, *, #1952, .F. ) ;
#10081 = PLANE ( 'NONE',  #7130 ) ;
#10082 = CARTESIAN_POINT ( 'NONE',  ( -13.67949125328055793, -52.30193472759165729, 56.95898663485335334 ) ) ;
#10083 = EDGE_CURVE ( 'NONE', #5848, #6974, #2304, .T. ) ;
#10084 = AXIS2_PLACEMENT_3D ( 'NONE', #8252, #3520, #14156 ) ;
#10086 = VECTOR ( 'NONE', #7906, 1000.000000000000000 ) ;
#10085 = DIRECTION ( 'NONE',  ( 0.000000000000000000, 1.224646799147350002E-16, -1.000000000000000000 ) ) ;
#10087 = LINE ( 'NONE', #4284, #14297 ) ;
#10088 = EDGE_CURVE ( 'NONE', #7300, #9964, #5651, .T. ) ;
#10089 = FACE_OUTER_BOUND ( 'NONE', #9582, .T. ) ;
#10090 = EDGE_CURVE ( 'NONE', #12240, #12386, #5809, .T. ) ;
#10091 = DIRECTION ( 'NONE',  ( 1.445602896647339656E-16, 0.000000000000000000, -1.000000000000000000 ) ) ;
#10092 = CARTESIAN_POINT ( 'NONE',  ( -38.20013690429809827, 4.873818854045000037, 20.51204286552489009 ) ) ;
#10093 = DIRECTION ( 'NONE',  ( -0.4224988092984258703, -0.5670050759397237128, -0.7071067811865479058 ) ) ;
#10094 = DIRECTION ( 'NONE',  ( 0.000000000000000000, 1.000000000000000000, 1.224646799147350002E-16 ) ) ;
#10095 = ORIENTED_EDGE ( 'NONE', *, *, #6848, .F. ) ;
#10097 = ORIENTED_EDGE ( 'NONE', *, *, #2874, .F. ) ;
#10096 = CARTESIAN_POINT ( 'NONE',  ( -23.59621936791819863, -19.33378413377805671, 56.85231026484398598 ) ) ;
#10098 = ORIENTED_EDGE ( 'NONE', *, *, #2334, .T. ) ;
#10099 = CARTESIAN_POINT ( 'NONE',  ( -18.09969986081100402, -109.6034951651679279, -1.661189050032654269 ) ) ;
#10101 = ORIENTED_EDGE ( 'NONE', *, *, #4108, .T. ) ;
#10100 = CARTESIAN_POINT ( 'NONE',  ( 1.817575469379459907, 10.05207975124035613, 16.39402607183602711 ) ) ;
#10102 = B_SPLINE_CURVE_WITH_KNOTS ( 'NONE', 3,
 ( #5724, #9315, #11616, #1132 ),
 .UNSPECIFIED., .F., .F.,
 ( 4, 4 ),
 ( 0.000000000000000000, 1.000000000000000000 ),
 .UNSPECIFIED. ) ;
#10103 = CARTESIAN_POINT ( 'NONE',  ( -15.49969986081099904, 4.873818854045000037, 24.21206422150099868 ) ) ;
#10104 = AXIS2_PLACEMENT_3D ( 'NONE', #3071, #12411, #1929 ) ;
#10105 = CARTESIAN_POINT ( 'NONE',  ( 21.85920135429435263, -27.00737899243800300, 27.46206422150099868 ) ) ;
#10106 =( LENGTH_UNIT ( ) NAMED_UNIT ( * ) SI_UNIT ( .MILLI., .METRE. ) );
#10107 = ADVANCED_FACE ( 'NONE', ( #11222 ), #739, .F. ) ;
#10108 = DIRECTION ( 'NONE',  ( 8.018662683283438208E-16, -5.975035461963189015E-16, -1.000000000000000000 ) ) ;
#10109 = AXIS2_PLACEMENT_3D ( 'NONE', #5989, #271, #8517 ) ;
#10110 = CARTESIAN_POINT ( 'NONE',  ( -15.49969986081092088, -13.50737899243822504, 57.00231026484397745 ) ) ;
#10111 = VERTEX_POINT ( 'NONE', #14738 ) ;
#10112 = CARTESIAN_POINT ( 'NONE',  ( -15.42470001081054498, -57.00737899243800655, 57.00223526506900384 ) ) ;
#10113 = ORIENTED_EDGE ( 'NONE', *, *, #7914, .T. ) ;
#10114 = DIRECTION ( 'NONE',  ( 0.000000000000000000, 9.130123557772668334E-17, -1.000000000000000000 ) ) ;
#10115 = EDGE_LOOP ( 'NONE', ( #14608, #14908, #7535, #3319 ) ) ;
#10116 = ORIENTED_EDGE ( 'NONE', *, *, #9809, .T. ) ;
#10117 = VECTOR ( 'NONE', #1877, 1000.000000000000227 ) ;
#10118 = CARTESIAN_POINT ( 'NONE',  ( -15.49969986081099904, -32.00737899243799944, 24.21206422150100224 ) ) ;
#10119 = ORIENTED_EDGE ( 'NONE', *, *, #13819, .T. ) ;
#10121 = ADVANCED_FACE ( 'NONE', ( #11291 ), #13093, .F. ) ;
#10120 = CARTESIAN_POINT ( 'NONE',  ( -9.481988904325579171, -39.22957468916221302, 56.51670373693783489 ) ) ;
#10122 = SURFACE_SIDE_STYLE ('',( #9199 ) ) ;
#10123 = DIRECTION ( 'NONE',  ( 0.5975035461963189576, 0.8018662683283437342, 0.000000000000000000 ) ) ;
#10124 = VECTOR ( 'NONE', #14837, 1000.000000000000000 ) ;
#10125 = CARTESIAN_POINT ( 'NONE',  ( 18.53245405280427960, -27.00737899243800300, 39.96206422150099513 ) ) ;
#10126 = UNCERTAINTY_MEASURE_WITH_UNIT (LENGTH_MEASURE( 1.000000000000000082E-05 ), #5799, 'distance_accuracy_value', 'NONE');
#10127 = LINE ( 'NONE', #5250, #4503 ) ;
#10129 = CARTESIAN_POINT ( 'NONE',  ( -35.80601265084589357, 12.32432269367079591, 32.26206422150099939 ) ) ;
#10128 = CARTESIAN_POINT ( 'NONE',  ( -12.87131257180735844, -22.19373785326158099, 57.00231026484399166 ) ) ;
#10130 = ORIENTED_EDGE ( 'NONE', *, *, #11585, .T. ) ;
#10131 = DIRECTION ( 'NONE',  ( 0.3533329742249643468, 0.9354976265738682573, -2.756373558169988945E-16 ) ) ;
#10132 = CARTESIAN_POINT ( 'NONE',  ( -12.25471857405102405, -7.219983152459794162, 56.85231026484398598 ) ) ;
#10133 = ORIENTED_EDGE ( 'NONE', *, *, #7294, .T. ) ;
#10134 = ORIENTED_EDGE ( 'NONE', *, *, #13187, .T. ) ;
#10135 = PLANE ( 'NONE',  #6391 ) ;
#10136 = CARTESIAN_POINT ( 'NONE',  ( -15.49969986081099727, -27.00737899243800300, 2.502310264843997878 ) ) ;
#10137 = DIRECTION ( 'NONE',  ( -0.9673062255102924389, 0.2536112499260064768, -9.271838545667833343E-16 ) ) ;
#10138 = EDGE_LOOP ( 'NONE', ( #11625, #4975, #12222, #14556 ) ) ;
#10139 = CARTESIAN_POINT ( 'NONE',  ( 13.85920135429429934, -27.00737899243800300, 21.71206422150100224 ) ) ;
#10140 = EDGE_CURVE ( 'NONE', #1022, #6106, #14385, .T. ) ;
#10141 = FACE_OUTER_BOUND ( 'NONE', #445, .T. ) ;
#10142 = DIRECTION ( 'NONE',  ( 3.002379285914464293E-17, -0.6316231926473815372, -0.7752755268354141194 ) ) ;
#10143 = LINE ( 'NONE', #8999, #12391 ) ;
#10144 = DIRECTION ( 'NONE',  ( 0.000000000000000000, 0.1872998510044759646, 0.9823027872370621028 ) ) ;
#10145 = LINE ( 'NONE', #904, #14281 ) ;
#10146 = ORIENTED_EDGE ( 'NONE', *, *, #11650, .F. ) ;
#10147 = DIRECTION ( 'NONE',  ( 0.5975035461963189576, 0.8018662683283437342, 0.000000000000000000 ) ) ;
#10148 = VECTOR ( 'NONE', #12687, 1000.000000000000114 ) ;
#10149 = CARTESIAN_POINT ( 'NONE',  ( -5.499699860811003482, -46.50737899243799944, 44.50231026484399877 ) ) ;
#10150 = ORIENTED_EDGE ( 'NONE', *, *, #14663, .F. ) ;
#10152 = VERTEX_POINT ( 'NONE', #316 ) ;
#10151 = LINE ( 'NONE', #13613, #9610 ) ;
#10153 = VERTEX_POINT ( 'NONE', #2679 ) ;
#10154 = ADVANCED_FACE ( 'NONE', ( #10867 ), #3105, .F. ) ;
#10155 = LINE ( 'NONE', #11466, #13494 ) ;
#10156 = CARTESIAN_POINT ( 'NONE',  ( -8.321349321884236261, -48.04850127655814873, 56.30906253082663682 ) ) ;
#10157 = ADVANCED_FACE ( 'NONE', ( #10936 ), #4259, .F. ) ;
#10158 = DIRECTION ( 'NONE',  ( 1.000000000000000000, 1.000000000000000078E-15, 1.000000000000000078E-15 ) ) ;
#10159 = DIRECTION ( 'NONE',  ( 0.5975035461963188466, 0.8018662683283438453, 0.000000000000000000 ) ) ;
#10160 = VECTOR ( 'NONE', #9019, 1000.000000000000114 ) ;
#10161 = LINE ( 'NONE', #1919, #8464 ) ;
#10162 = B_SPLINE_CURVE_WITH_KNOTS ( 'NONE', 3,
 ( #7889, #4464, #13718, #11269, #2170, #12424, #14866, #1940, #1091, #7808, #948, #12657, #4390, #14790, #12495, #2016, #4539, #6665, #11572, #13797, #11348, #5526, #9042, #12580, #3315, #7962, #6816, #13870, #11495, #10346 ),
 .UNSPECIFIED., .F., .F.,
 ( 4, 2, 2, 2, 2, 2, 2, 2, 2, 2, 2, 2, 2, 2, 4 ),
 ( 0.01102539692970626664, 0.01171599123889527534, 0.01240658554808428231, 0.01309717985727329101, 0.01378777416646229798, 0.01447836847565130668, 0.01516896278484031538, 0.01655015140321834666, 0.01793134002159637447, 0.01862193433078539531, 0.01931252863997440922, 0.02000312294916342659, 0.02069371725835244050, 0.02138431156754145440, 0.02207490587673047178 ),
 .UNSPECIFIED. ) ;
#10163 = LINE ( 'NONE', #14840, #10160 ) ;
#10164 = CARTESIAN_POINT ( 'NONE',  ( -15.49969986081091733, -13.50737899243822682, 54.00231026484399166 ) ) ;
#10165 = DIRECTION ( 'NONE',  ( -8.018662683283438208E-16, 5.975035461963189015E-16, 1.000000000000000000 ) ) ;
#10166 = ORIENTED_EDGE ( 'NONE', *, *, #11051, .F. ) ;
#10167 = CARTESIAN_POINT ( 'NONE',  ( -15.57469986081099478, -23.50709773848280904, 54.00231026484400587 ) ) ;
#10168 = AXIS2_PLACEMENT_3D ( 'NONE', #11453, #6618, #7922 ) ;
#10169 = EDGE_LOOP ( 'NONE', ( #12900, #9447, #5394, #3305 ) ) ;
#10170 = SHAPE_REPRESENTATION ( 'Insert Torx Screw', ( #6789 ), #4860 ) ;
#10172 = EDGE_LOOP ( 'NONE', ( #7158, #3373, #646, #6104 ) ) ;
#10171 = CARTESIAN_POINT ( 'NONE',  ( -15.49968909271368211, -3.507379016232285096, 61.71092834827113194 ) ) ;
#10173 = EDGE_LOOP ( 'NONE', ( #6257, #9180, #14255, #1930 ) ) ;
#10174 = EDGE_CURVE ( 'NONE', #11198, #11272, #783, .T. ) ;
#10175 = CARTESIAN_POINT ( 'NONE',  ( -13.18491133144367211, -15.23222315862922827, 56.89875687425072215 ) ) ;
#10176 = ADVANCED_FACE ( 'NONE', ( #13246 ), #5181, .T. ) ;
#10177 = VERTEX_POINT ( 'NONE', #14812 ) ;
#10178 = AXIS2_PLACEMENT_3D ( 'NONE', #873, #11646, #5679 ) ;
#10179 = CYLINDRICAL_SURFACE ( 'NONE', #8535, 3.000000000000002665 ) ;
#10180 = EDGE_CURVE ( 'NONE', #6478, #13190, #12448, .T. ) ;
#10181 = VECTOR ( 'NONE', #6311, 1000.000000000000000 ) ;
#10182 = DIRECTION ( 'NONE',  ( 0.000000000000000000, 0.000000000000000000, -1.000000000000000000 ) ) ;
#10183 = AXIS2_PLACEMENT_3D ( 'NONE', #11143, #1728, #10914 ) ;
#10184 = EDGE_CURVE ( 'NONE', #1107, #3863, #1782, .T. ) ;
#10185 = ORIENTED_EDGE ( 'NONE', *, *, #11975, .F. ) ;
#10186 = CARTESIAN_POINT ( 'NONE',  ( -22.04595456446742929, -18.23578246029658345, 56.85231026484398598 ) ) ;
#10187 =( GEOMETRIC_REPRESENTATION_CONTEXT ( 3 ) GLOBAL_UNCERTAINTY_ASSIGNED_CONTEXT ( ( #2654 ) ) GLOBAL_UNIT_ASSIGNED_CONTEXT ( ( #9849, #14517, #6167 ) ) REPRESENTATION_CONTEXT ( 'NONE', 'WORKASPACE' ) );
#10188 = CARTESIAN_POINT ( 'NONE',  ( -15.49969986081092088, -13.50737899243822504, 57.00231026484397745 ) ) ;
#10189 = EDGE_LOOP ( 'NONE', ( #1211, #14860, #5547, #2364 ) ) ;
#10190 = CARTESIAN_POINT ( 'NONE',  ( -1.508527451664999575, -46.50737899243799234, -6.997689735156000346 ) ) ;
#10191 = ORIENTED_EDGE ( 'NONE', *, *, #7785, .T. ) ;
#10192 = DIRECTION ( 'NONE',  ( 1.445602896647337931E-16, 0.000000000000000000, -1.000000000000000000 ) ) ;
#10193 = ORIENTED_EDGE ( 'NONE', *, *, #3115, .F. ) ;
#10194 = VERTEX_POINT ( 'NONE', #8485 ) ;
#10195 = CARTESIAN_POINT ( 'NONE',  ( 2.500300139188996518, -41.82625798755428548, 52.39987856403597988 ) ) ;
#10196 = ADVANCED_FACE ( 'NONE', ( #1965 ), #10135, .F. ) ;
#10197 = EDGE_CURVE ( 'NONE', #9374, #12241, #2129, .T. ) ;
#10198 = VERTEX_POINT ( 'NONE', #7333 ) ;
#10199 = VECTOR ( 'NONE', #10934, 999.9999999999998863 ) ;
#10200 = VECTOR ( 'NONE', #7666, 1000.000000000000000 ) ;
#10201 = CARTESIAN_POINT ( 'NONE',  ( -16.42437072798637843, -22.03270794722917714, 56.85231026484400019 ) ) ;
#10202 = AXIS2_PLACEMENT_3D ( 'NONE', #6077, #10764, #12066 ) ;
#10203 = FACE_OUTER_BOUND ( 'NONE', #11381, .T. ) ;
#10204 = CARTESIAN_POINT ( 'NONE',  ( -13.95777467540137806, -22.45074059323463089, 56.85231026484400019 ) ) ;
#10205 = CARTESIAN_POINT ( 'NONE',  ( 15.84215789323456569, -24.14741025098728144, 3.617636113674804310 ) ) ;
#10206 = AXIS2_PLACEMENT_3D ( 'NONE', #1921, #6792, #14772 ) ;
#10207 = EDGE_CURVE ( 'NONE', #6401, #13230, #8841, .T. ) ;
#10208 = CARTESIAN_POINT ( 'NONE',  ( 2.500300139188999182, -46.50737899243799944, -5.497689735156002122 ) ) ;
#10210 = LINE ( 'NONE', #4553, #3130 ) ;
#10209 = DIRECTION ( 'NONE',  ( 0.000000000000000000, 1.000000000000000000, 1.224646799147350002E-16 ) ) ;
#10211 = ORIENTED_EDGE ( 'NONE', *, *, #14593, .T. ) ;
#10212 = CARTESIAN_POINT ( 'NONE',  ( -10.16926643994361967, -19.57302854922115287, 57.00231026484399166 ) ) ;
#10213 = CARTESIAN_POINT ( 'NONE',  ( -19.38713143869018296, -6.429305403720261936, 56.85231026484398598 ) ) ;
#10214 = ORIENTED_EDGE ( 'NONE', *, *, #11305, .T. ) ;
#10215 = ORIENTED_EDGE ( 'NONE', *, *, #5926, .F. ) ;
#10216 = DIRECTION ( 'NONE',  ( -0.3204693369899890287, -0.9472588896649093426, 3.090169943749498472E-16 ) ) ;
#10217 = CARTESIAN_POINT ( 'NONE',  ( -15.49969986081099727, -52.50737899243799944, 2.502310264843994769 ) ) ;
#10218 = CARTESIAN_POINT ( 'NONE',  ( -18.15085299098534222, -14.64962258016358376, 51.25231026484399166 ) ) ;
#10219 = LINE ( 'NONE', #14894, #3018 ) ;
#10220 = VERTEX_POINT ( 'NONE', #13818 ) ;
#10221 = DIRECTION ( 'NONE',  ( 0.000000000000000000, 0.000000000000000000, -1.000000000000000000 ) ) ;
#10222 = VECTOR ( 'NONE', #3628, 1000.000000000000114 ) ;
#10223 = AXIS2_PLACEMENT_3D ( 'NONE', #7538, #1729, #13594 ) ;
#10224 = LINE ( 'NONE', #7992, #2190 ) ;
#10225 = CONTEXT_DEPENDENT_SHAPE_REPRESENTATION ( #7418, #8591 ) ;
#10226 = CARTESIAN_POINT ( 'NONE',  ( -7.629407442448590260, -48.55937836028767407, 20.93097002895218495 ) ) ;
#10227 = VECTOR ( 'NONE', #5789, 1000.000000000000000 ) ;
#10228 = B_SPLINE_CURVE_WITH_KNOTS ( 'NONE', 3,
 ( #12010, #9555, #6251, #13018, #9481, #14450, #4824, #6181, #14231, #10933, #3748, #10863, #13242, #3674, #12943, #14306, #2523, #8405, #1452, #8481, #390, #5050, #5121, #14382, #3898, #8557 ),
 .UNSPECIFIED., .F., .F.,
 ( 4, 2, 2, 2, 2, 2, 2, 2, 2, 2, 2, 2, 4 ),
 ( 0.03783278222213234954, 0.03940995139284290266, 0.04019853597819818269, 0.04098712056355345579, 0.04177570514890873582, 0.04256428973426400891, 0.04414145890497456204, 0.04493004349032983513, 0.04571862807568510823, 0.04729579724639566135, 0.04808438183175094138, 0.04887296641710622142, 0.05045013558781678148 ),
 .UNSPECIFIED. ) ;
#10229 = AXIS2_PLACEMENT_3D ( 'NONE', #330, #1157, #4688 ) ;
#10230 = ADVANCED_FACE ( 'NONE', ( #10444 ), #5770, .F. ) ;
#10231 = CARTESIAN_POINT ( 'NONE',  ( -15.49969986081091378, -13.50737899243822859, 51.00231026484399166 ) ) ;
#10232 = CARTESIAN_POINT ( 'NONE',  ( 2.377116011596400291, -23.18484177525213141, -8.848022433876742809 ) ) ;
#10233 = ORIENTED_EDGE ( 'NONE', *, *, #9107, .T. ) ;
#10234 = CARTESIAN_POINT ( 'NONE',  ( -10.73868464545405921, -90.63222195594610753, -2.967393652951166860 ) ) ;
#10235 = DIRECTION ( 'NONE',  ( -0.1165201156931293391, -0.9931883319083343320, 4.999999999999998416E-16 ) ) ;
#10236 = CARTESIAN_POINT ( 'NONE',  ( -15.49969986081100082, 22.99262100756200411, 8.337064221501000461 ) ) ;
#10237 = EDGE_LOOP ( 'NONE', ( #12494, #6472, #10824, #11273, #13857 ) ) ;
#10238 = CARTESIAN_POINT ( 'NONE',  ( -7.517316220913920155, -45.05891496665708473, 46.54929868018043493 ) ) ;
#10239 = EDGE_LOOP ( 'NONE', ( #8079, #10487, #2171, #8897 ) ) ;
#10240 = CARTESIAN_POINT ( 'NONE',  ( -15.49969986081092088, -13.50737899243822504, 56.85231026484398598 ) ) ;
#10241 = CARTESIAN_POINT ( 'NONE',  ( -15.49969986081099904, 20.99262100756200056, 16.16206422150100153 ) ) ;
#10242 = VECTOR ( 'NONE', #6203, 1000.000000000000000 ) ;
#10243 = AXIS2_PLACEMENT_3D ( 'NONE', #10907, #6226, #13219 ) ;
#10244 = CARTESIAN_POINT ( 'NONE',  ( 2.500300139188999182, -46.50737899243799944, 19.50231026484399877 ) ) ;
#10245 = DIRECTION ( 'NONE',  ( -0.9966498018049937402, 0.08178736187251965661, -8.480480961564258050E-16 ) ) ;
#10246 = LINE ( 'NONE', #9168, #4816 ) ;
#10247 = EDGE_CURVE ( 'NONE', #12486, #13092, #15035, .T. ) ;
#10248 = DIRECTION ( 'NONE',  ( 0.000000000000000000, 0.000000000000000000, 1.000000000000000000 ) ) ;
#10249 = LINE ( 'NONE', #11474, #10707 ) ;
#10250 = AXIS2_PLACEMENT_3D ( 'NONE', #9762, #1723, #4248 ) ;
#10251 = FACE_OUTER_BOUND ( 'NONE', #1081, .T. ) ;
#10252 = EDGE_LOOP ( 'NONE', ( #9296, #3164, #14367, #2022, #3540, #5416, #13782, #661 ) ) ;
#10253 = DIRECTION ( 'NONE',  ( -0.8018662683283436232, 0.5975035461963189576, -9.999999999999998805E-16 ) ) ;
#10254 = EDGE_LOOP ( 'NONE', ( #13059, #2621, #675, #49 ) ) ;
#10256 = VERTEX_POINT ( 'NONE', #5548 ) ;
#10255 = CARTESIAN_POINT ( 'NONE',  ( -25.48037379874287467, -12.85419436533228144, 60.35950308624435934 ) ) ;
#10257 = ORIENTED_EDGE ( 'NONE', *, *, #12945, .F. ) ;
#10258 = APPLICATION_CONTEXT ( 'automotive_design' ) ;
#10259 = VECTOR ( 'NONE', #5594, 1000.000000000000000 ) ;
#10260 = DIRECTION ( 'NONE',  ( 1.000000000000000000, 1.201369187114119994E-15, 9.616040805000176517E-16 ) ) ;
#10261 = VERTEX_POINT ( 'NONE', #12602 ) ;
#10262 = LINE ( 'NONE', #3382, #2680 ) ;
#10263 = CARTESIAN_POINT ( 'NONE',  ( -22.67472226038933059, -17.21206232108429290, 57.00231026484397745 ) ) ;
#10264 = ADVANCED_FACE ( 'NONE', ( #11665 ), #3413, .F. ) ;
#10265 = AXIS2_PLACEMENT_3D ( 'NONE', #7958, #1012, #5670 ) ;
#10266 =( BOUNDED_CURVE ( )  B_SPLINE_CURVE ( 3, ( #10460, #4727, #2357, #14056 ),
 .UNSPECIFIED., .F., .T. ) 
 B_SPLINE_CURVE_WITH_KNOTS ( ( 4, 4 ),
 ( 3.141592653589793116, 4.712388980384689674 ),
 .UNSPECIFIED. ) 
 CURVE ( )  GEOMETRIC_REPRESENTATION_ITEM ( )  RATIONAL_B_SPLINE_CURVE ( ( 1.000000000000000000, 0.8047378541243649375, 0.8047378541243649375, 1.000000000000000000 ) ) 
 REPRESENTATION_ITEM ( '' )  );
#10267 = EDGE_LOOP ( 'NONE', ( #4431, #12256, #12575, #11499 ) ) ;
#10268 = CARTESIAN_POINT ( 'NONE',  ( -19.73323262537018508, -51.30037923254471366, -17.75858867747328418 ) ) ;
#10269 = ADVANCED_FACE ( 'NONE', ( #11442 ), #9082, .T. ) ;
#10270 = ORIENTED_EDGE ( 'NONE', *, *, #12152, .T. ) ;
#10271 = CARTESIAN_POINT ( 'NONE',  ( -17.05536012119625866, -6.605120582739408164, 57.00231026484397745 ) ) ;
#10272 = ORIENTED_EDGE ( 'NONE', *, *, #13085, .F. ) ;
#10273 = DIRECTION ( 'NONE',  ( -0.4177292884839972076, -0.9085715390340231012, 2.079116908177588539E-16 ) ) ;
#10274 = ORIENTED_EDGE ( 'NONE', *, *, #9844, .T. ) ;
#10275 = ORIENTED_EDGE ( 'NONE', *, *, #14873, .F. ) ;
#10276 = LINE ( 'NONE', #2249, #12505 ) ;
#10277 = ORIENTED_EDGE ( 'NONE', *, *, #11677, .T. ) ;
#10278 = ADVANCED_FACE ( 'NONE', ( #9293 ), #14951, .T. ) ;
#10279 = CARTESIAN_POINT ( 'NONE',  ( -8.324915140515775747, -40.95899558977754396, 56.30975957592992387 ) ) ;
#10280 = PLANE ( 'NONE',  #12219 ) ;
#10281 = CARTESIAN_POINT ( 'NONE',  ( -15.49969986081092088, -13.50737899243822504, 57.00231026484397745 ) ) ;
#10282 = EDGE_CURVE ( 'NONE', #11225, #569, #3335, .T. ) ;
#10283 = ADVANCED_FACE ( 'NONE', ( #2038 ), #15110, .F. ) ;
#10284 = AXIS2_PLACEMENT_3D ( 'NONE', #14336, #4565, #9217 ) ;
#10286 = PLANE ( 'NONE',  #11937 ) ;
#10285 = FACE_OUTER_BOUND ( 'NONE', #14875, .T. ) ;
#10287 = ORIENTED_EDGE ( 'NONE', *, *, #568, .F. ) ;
#10288 = DIRECTION ( 'NONE',  ( 0.000000000000000000, 0.000000000000000000, -1.000000000000000000 ) ) ;
#10289 = CARTESIAN_POINT ( 'NONE',  ( -16.95106854142316877, -17.77697586203957059, -13.26081966632196263 ) ) ;
#10290 = VERTEX_POINT ( 'NONE', #4413 ) ;
#10291 = VERTEX_POINT ( 'NONE', #3485 ) ;
#10292 = CARTESIAN_POINT ( 'NONE',  ( -12.91190996461674168, -5.858263458394094236, 56.85231026484398598 ) ) ;
#10293 = CARTESIAN_POINT ( 'NONE',  ( -21.85724566142533121, -39.62315458006131053, -17.45603278757056387 ) ) ;
#10294 = CARTESIAN_POINT ( 'NONE',  ( -5.499699860810997265, -46.50737899243799944, -7.997689735156003010 ) ) ;
#10295 = ORIENTED_EDGE ( 'NONE', *, *, #13526, .T. ) ;
#10296 = DIRECTION ( 'NONE',  ( -0.1908089953765445546, 0.4456494155713290328, -0.8746362247725203432 ) ) ;
#10297 = PRODUCT ( 'MAS-672', 'MAS-672', '', ( #5555 ) ) ;
#10298 = VECTOR ( 'NONE', #4290, 1000.000000000000114 ) ;
#10299 = DIRECTION ( 'NONE',  ( 0.9999272109403024578, -0.01206535623791937274, 8.090169943749475688E-16 ) ) ;
#10300 = DIRECTION ( 'NONE',  ( -0.4587843131450244361, 0.8885476655824651182, -8.987940462991669572E-16 ) ) ;
#10301 = EDGE_CURVE ( 'NONE', #9733, #2288, #8114, .T. ) ;
#10302 = CARTESIAN_POINT ( 'NONE',  ( -15.49969986081092088, -13.50737899243822504, 57.00231026484397745 ) ) ;
#10303 = LINE ( 'NONE', #12611, #3780 ) ;
#10304 = AXIS2_PLACEMENT_3D ( 'NONE', #3397, #11501, #12737 ) ;
#10305 = ADVANCED_FACE ( 'NONE', ( #8062 ), #50, .T. ) ;
#10306 = ORIENTED_EDGE ( 'NONE', *, *, #14539, .F. ) ;
#10307 = FACE_OUTER_BOUND ( 'NONE', #13, .T. ) ;
#10308 = CARTESIAN_POINT ( 'NONE',  ( -9.508527451664997798, -48.50737899243800655, -5.497689735156000346 ) ) ;
#10309 = DIRECTION ( 'NONE',  ( -1.000000000000000000, -1.000000000000000078E-15, -1.000000000000000078E-15 ) ) ;
#10310 = CIRCLE ( 'NONE', #3720, 9.974999999999999645 ) ;
#10311 = CONICAL_SURFACE ( 'NONE', #3721, 15.87500000000000355, 0.1448623279155291654 ) ;
#10312 = DIRECTION ( 'NONE',  ( -8.018662683283439195E-16, 5.975035461963190001E-16, 1.000000000000000000 ) ) ;
#10313 = ORIENTED_EDGE ( 'NONE', *, *, #7269, .T. ) ;
#10314 = DIRECTION ( 'NONE',  ( 0.02283895005205794151, -0.9997391571607663341, 6.156614753256579139E-16 ) ) ;
#10315 = ORIENTED_EDGE ( 'NONE', *, *, #8362, .T. ) ;
#10316 = CARTESIAN_POINT ( 'NONE',  ( -22.08930316869620825, -18.17457871440291228, 57.00231026484397745 ) ) ;
#10317 = DIRECTION ( 'NONE',  ( 0.000000000000000000, 1.224646799147350002E-16, -1.000000000000000000 ) ) ;
#10318 = ADVANCED_FACE ( 'NONE', ( #12676 ), #9066, .F. ) ;
#10319 = DIRECTION ( 'NONE',  ( 0.000000000000000000, -1.850371707708594563E-16, 1.000000000000000000 ) ) ;
#10320 = CARTESIAN_POINT ( 'NONE',  ( -8.885611223908250977, -49.00780472460828463, 44.84073519055883139 ) ) ;
#10321 = AXIS2_PLACEMENT_3D ( 'NONE', #7081, #14065, #4510 ) ;
#10322 = AXIS2_PLACEMENT_3D ( 'NONE', #180, #14174, #12963 ) ;
#10323 = CARTESIAN_POINT ( 'NONE',  ( -12.38873450203231030, -7.152605626181999909, 56.85231026484398598 ) ) ;
#10324 = LINE ( 'NONE', #5801, #6484 ) ;
#10325 = CARTESIAN_POINT ( 'NONE',  ( -36.81467648506759360, -37.29975643136121022, 50.35554694645792040 ) ) ;
#10326 = DIRECTION ( 'NONE',  ( 1.000000000000000000, -1.291538348938060198E-32, 1.054621095516909827E-16 ) ) ;
#10327 = EDGE_LOOP ( 'NONE', ( #6315, #14630, #4262, #624, #1362, #7635, #9807, #8060, #8096, #9898, #13241, #14528, #8117, #888, #14699, #7828, #14259, #8142, #6259, #4149, #8427, #13959, #9355, #3184, #14776, #9060, #10214 ) ) ;
#10328 = CARTESIAN_POINT ( 'NONE',  ( 18.47600606207883445, -27.91756206037096888, 40.08355722636073182 ) ) ;
#10329 = EDGE_LOOP ( 'NONE', ( #11491, #2232, #8936, #11576 ) ) ;
#10331 = ORIENTED_EDGE ( 'NONE', *, *, #214, .F. ) ;
#10330 = CARTESIAN_POINT ( 'NONE',  ( -23.43779763612971223, -7.414416043088839281, 60.86287324052170078 ) ) ;
#10332 = ORIENTED_EDGE ( 'NONE', *, *, #6340, .F. ) ;
#10333 = VECTOR ( 'NONE', #2682, 1000.000000000000000 ) ;
#10334 = PLANE ( 'NONE',  #1655 ) ;
#10335 = ORIENTED_EDGE ( 'NONE', *, *, #388, .T. ) ;
#10336 = DIRECTION ( 'NONE',  ( 0.000000000000000000, -1.000000000000000000, -1.224646799147350002E-16 ) ) ;
#10337 = EDGE_CURVE ( 'NONE', #4677, #7227, #12525, .T. ) ;
#10338 = LINE ( 'NONE', #10263, #256 ) ;
#10339 =( LENGTH_UNIT ( ) NAMED_UNIT ( * ) SI_UNIT ( .MILLI., .METRE. ) );
#10340 = CIRCLE ( 'NONE', #3758, 2.458500000000002572 ) ;
#10341 = AXIS2_PLACEMENT_3D ( 'NONE', #2657, #14362, #8461 ) ;
#10342 = AXIS2_PLACEMENT_3D ( 'NONE', #9373, #13739, #4482 ) ;
#10343 = ORIENTED_EDGE ( 'NONE', *, *, #10894, .T. ) ;
#10344 = CARTESIAN_POINT ( 'NONE',  ( -20.77774051523950050, -50.52488293980518108, -17.62495337501153259 ) ) ;
#10345 = ORIENTED_EDGE ( 'NONE', *, *, #5905, .F. ) ;
#10346 = CARTESIAN_POINT ( 'NONE',  ( 14.68618260102869932, -27.00737899243800300, 46.46206422150099513 ) ) ;
#10347 = ORIENTED_EDGE ( 'NONE', *, *, #9802, .T. ) ;
#10348 = CARTESIAN_POINT ( 'NONE',  ( -15.49969986081100082, -19.50737899243800300, 19.50231026484399877 ) ) ;
#10349 = ORIENTED_EDGE ( 'NONE', *, *, #1650, .F. ) ;
#10350 = ORIENTED_EDGE ( 'NONE', *, *, #13605, .T. ) ;
#10351 = CARTESIAN_POINT ( 'NONE',  ( -9.251715890255169938, -8.391880844292892050, 56.85231026484398598 ) ) ;
#10352 = CYLINDRICAL_SURFACE ( 'NONE', #5662, 22.99999999999999645 ) ;
#10353 = ORIENTED_EDGE ( 'NONE', *, *, #6357, .T. ) ;
#10354 = CARTESIAN_POINT ( 'NONE',  ( -23.04246617642294837, -20.11702390495540982, 56.23888206045033655 ) ) ;
#10355 = AXIS2_PLACEMENT_3D ( 'NONE', #2396, #7477, #14448 ) ;
#10356 = ADVANCED_FACE ( 'NONE', ( #8143 ), #6911, .F. ) ;
#10357 = EDGE_CURVE ( 'NONE', #8706, #4315, #12834, .T. ) ;
#10358 = CARTESIAN_POINT ( 'NONE',  ( -18.09969986081100402, -102.4362639876081289, -6.675878016713550522 ) ) ;
#10359 = VECTOR ( 'NONE', #586, 1000.000000000000000 ) ;
#10360 = VECTOR ( 'NONE', #11235, 1000.000000000000114 ) ;
#10361 = DIRECTION ( 'NONE',  ( 0.000000000000000000, 0.1872998510044759646, 0.9823027872370621028 ) ) ;
#10363 = CARTESIAN_POINT ( 'NONE',  ( -8.701256315749452241, -15.46758698257906950, 56.85231026484400019 ) ) ;
#10362 = DIRECTION ( 'NONE',  ( -1.000000000000000000, 0.000000000000000000, 0.000000000000000000 ) ) ;
#10364 = ORIENTED_EDGE ( 'NONE', *, *, #6659, .T. ) ;
#10365 = CARTESIAN_POINT ( 'NONE',  ( -15.49969986081099904, 13.89262100756199736, 29.46206422150100224 ) ) ;
#10366 = CARTESIAN_POINT ( 'NONE',  ( -15.49969986081099904, -37.00737899243799944, 19.50231026484400232 ) ) ;
#10367 = ORIENTED_EDGE ( 'NONE', *, *, #9969, .T. ) ;
#10368 = ORIENTED_EDGE ( 'NONE', *, *, #2556, .T. ) ;
#10369 = DIRECTION ( 'NONE',  ( 9.912705577010322591E-16, -0.1872998510044552312, -0.9823027872370662106 ) ) ;
#10370 = CARTESIAN_POINT ( 'NONE',  ( -16.55105184719503697, -36.57242519587391172, -17.98385852237137428 ) ) ;
#10371 = DIRECTION ( 'NONE',  ( 0.9437508163134050720, 0.3306575217771122732, 5.591929034707472732E-16 ) ) ;
#10372 = ORIENTED_EDGE ( 'NONE', *, *, #5868, .F. ) ;
#10373 = PLANE ( 'NONE',  #1504 ) ;
#10374 = EDGE_CURVE ( 'NONE', #8446, #12112, #10673, .T. ) ;
#10375 = ADVANCED_FACE ( 'NONE', ( #14275 ), #9376, .F. ) ;
#10376 =( GEOMETRIC_REPRESENTATION_CONTEXT ( 3 ) GLOBAL_UNCERTAINTY_ASSIGNED_CONTEXT ( ( #370 ) ) GLOBAL_UNIT_ASSIGNED_CONTEXT ( ( #958, #13884, #5535 ) ) REPRESENTATION_CONTEXT ( 'NONE', 'WORKASPACE' ) );
#10377 = EDGE_CURVE ( 'NONE', #7809, #4749, #5591, .T. ) ;
#10378 = DIRECTION ( 'NONE',  ( 0.000000000000000000, 0.1872998510044689147, 0.9823027872370635460 ) ) ;
#10379 = ITEM_DEFINED_TRANSFORMATION ( 'NONE', 'NONE', #13185,  #6789 ) ;
#10380 = DIRECTION ( 'NONE',  ( -1.000000000000000000, 1.499759782661860071E-32, -1.224646799147350002E-16 ) ) ;
#10381 = EDGE_CURVE ( 'NONE', #7723, #8731, #14496, .T. ) ;
#10382 = FACE_OUTER_BOUND ( 'NONE', #4353, .T. ) ;
#10383 = LINE ( 'NONE', #10531, #12553 ) ;
#10384 = ORIENTED_EDGE ( 'NONE', *, *, #8776, .F. ) ;
#10385 = CARTESIAN_POINT ( 'NONE',  ( -15.49969986081093509, -96.50737899243799234, -0.1262635860074601546 ) ) ;
#10386 = DIRECTION ( 'NONE',  ( 0.000000000000000000, 0.000000000000000000, -1.000000000000000000 ) ) ;
#10387 = DIRECTION ( 'NONE',  ( 0.8018662683283437342, -0.5975035461963188466, 9.999999999999996833E-16 ) ) ;
#10388 = LINE ( 'NONE', #2287, #8529 ) ;
#10389 = ORIENTED_EDGE ( 'NONE', *, *, #2459, .T. ) ;
#10390 = CARTESIAN_POINT ( 'NONE',  ( -15.49969986081099904, 71.39262100756199914, 24.21206422150100579 ) ) ;
#10391 = VERTEX_POINT ( 'NONE', #13354 ) ;
#10392 = LINE ( 'NONE', #8242, #5426 ) ;
#10393 = DIRECTION ( 'NONE',  ( -8.018662683283438208E-16, 5.975035461963189015E-16, 1.000000000000000000 ) ) ;
#10394 = EDGE_CURVE ( 'NONE', #13305, #1644, #12202, .T. ) ;
#10395 = CARTESIAN_POINT ( 'NONE',  ( -7.886584594865169606, -46.96511696614940234, 21.96004823855531640 ) ) ;
#10396 = CARTESIAN_POINT ( 'NONE',  ( -7.796873843965146378, -46.67446211046079441, 47.00231026484400587 ) ) ;
#10397 = PLANE ( 'NONE',  #178 ) ;
#10398 = AXIS2_PLACEMENT_3D ( 'NONE', #11909, #1433, #3875 ) ;
#10399 = DIRECTION ( 'NONE',  ( -8.018662683283438208E-16, 5.975035461963189015E-16, 1.000000000000000000 ) ) ;
#10400 = CARTESIAN_POINT ( 'NONE',  ( 9.000300139189000959, -19.50737899243800300, 52.60220335465780295 ) ) ;
#10401 = ADVANCED_FACE ( 'NONE', ( #7600 ), #1023, .F. ) ;
#10402 = CARTESIAN_POINT ( 'NONE',  ( -15.49969986081092088, -13.50737899243822504, 57.00231026484397745 ) ) ;
#10403 = ORIENTED_EDGE ( 'NONE', *, *, #13424, .F. ) ;
#10404 = DIRECTION ( 'NONE',  ( 0.5196486895212314439, -0.8543800322332368857, 9.271838545667882647E-16 ) ) ;
#10405 = ORIENTED_EDGE ( 'NONE', *, *, #5882, .T. ) ;
#10406 = LINE ( 'NONE', #12483, #5301 ) ;
#10408 = ORIENTED_EDGE ( 'NONE', *, *, #1535, .F. ) ;
#10407 = CARTESIAN_POINT ( 'NONE',  ( -18.50396719079564889, -6.011671700261853601, 56.85231026484398598 ) ) ;
#10409 = ORIENTED_EDGE ( 'NONE', *, *, #8152, .T. ) ;
#10410 = CARTESIAN_POINT ( 'NONE',  ( -15.49969986081099549, 2.992621007561993451, 52.21206422150100224 ) ) ;
#10411 = EDGE_LOOP ( 'NONE', ( #5636, #2526, #9411, #2567 ) ) ;
#10412 = VECTOR ( 'NONE', #6791, 1000.000000000000000 ) ;
#10413 = DIRECTION ( 'NONE',  ( -8.018662683283438208E-16, 5.975035461963189015E-16, 1.000000000000000000 ) ) ;
#10414 = DIRECTION ( 'NONE',  ( -1.000000000000000078E-15, 1.000000000000000000, 0.000000000000000000 ) ) ;
#10415 = CARTESIAN_POINT ( 'NONE',  ( -8.525484111995742964, -7.700351810740323266, 56.85231026484400019 ) ) ;
#10416 =( NAMED_UNIT ( * ) SI_UNIT ( $, .STERADIAN. ) SOLID_ANGLE_UNIT ( ) );
#10417 = VECTOR ( 'NONE', #8496, 1000.000000000000000 ) ;
#10418 = ADVANCED_FACE ( 'NONE', ( #13948 ), #2984, .F. ) ;
#10419 = FACE_BOUND ( 'NONE', #13058, .T. ) ;
#10420 = EDGE_LOOP ( 'NONE', ( #7505, #2866, #12353, #5242, #2904, #465, #8105, #6209 ) ) ;
#10421 = CARTESIAN_POINT ( 'NONE',  ( -20.61203582816999713, -106.9749035585825681, -5.105386947918939100 ) ) ;
#10422 = VERTEX_POINT ( 'NONE', #13651 ) ;
#10423 = DIRECTION ( 'NONE',  ( -8.018662683283438208E-16, 5.975035461963189015E-16, 1.000000000000000000 ) ) ;
#10424 = ORIENTED_EDGE ( 'NONE', *, *, #5012, .F. ) ;
#10425 = CIRCLE ( 'NONE', #10922, 9.974999999999999645 ) ;
#10426 = ORIENTED_EDGE ( 'NONE', *, *, #4113, .T. ) ;
#10427 = CARTESIAN_POINT ( 'NONE',  ( -14.61203582817000246, -106.9748017008338365, -5.104852750214475599 ) ) ;
#10428 = VERTEX_POINT ( 'NONE', #8275 ) ;
#10429 = CARTESIAN_POINT ( 'NONE',  ( -20.69159174768329379, -22.05612254491840218, 56.64242933135466274 ) ) ;
#10430 = AXIS2_PLACEMENT_3D ( 'NONE', #10630, #13167, #6023 ) ;
#10431 = LINE ( 'NONE', #13953, #6579 ) ;
#10432 = CARTESIAN_POINT ( 'NONE',  ( -10.12832823130355209, -90.53875328855629334, -5.525617877236590481 ) ) ;
#10433 = CONICAL_SURFACE ( 'NONE', #14838, 3.000000000000002665, 1.047197551196598297 ) ;
#10434 = CYLINDRICAL_SURFACE ( 'NONE', #8893, 4.499999999999999112 ) ;
#10435 = EDGE_CURVE ( 'NONE', #4771, #10220, #14029, .T. ) ;
#10437 = DIRECTION ( 'NONE',  ( -0.9983330752162417054, -0.05771543059946733500, -7.660444431189782383E-16 ) ) ;
#10436 = DIRECTION ( 'NONE',  ( -8.018662683283439195E-16, 5.975035461963190001E-16, 1.000000000000000000 ) ) ;
#10438 = ORIENTED_EDGE ( 'NONE', *, *, #4912, .T. ) ;
#10439 = DIRECTION ( 'NONE',  ( 0.000000000000000000, 0.1872998510044759646, 0.9823027872370621028 ) ) ;
#10440 = AXIS2_PLACEMENT_3D ( 'NONE', #8635, #7627, #1745 ) ;
#10441 = CARTESIAN_POINT ( 'NONE',  ( -15.49969986081091022, -13.50737899243823215, 46.00231026484398456 ) ) ;
#10442 = ORIENTED_EDGE ( 'NONE', *, *, #8228, .T. ) ;
#10443 = ORIENTED_EDGE ( 'NONE', *, *, #4575, .T. ) ;
#10444 = FACE_OUTER_BOUND ( 'NONE', #5525, .T. ) ;
#10445 = EDGE_CURVE ( 'NONE', #13341, #11896, #7275, .T. ) ;
#10446 = AXIS2_PLACEMENT_3D ( 'NONE', #6846, #12842, #11605 ) ;
#10447 = FACE_OUTER_BOUND ( 'NONE', #9693, .T. ) ;
#10448 = EDGE_LOOP ( 'NONE', ( #12183, #5622, #13446, #11069 ) ) ;
#10449 = CARTESIAN_POINT ( 'NONE',  ( -18.09969986081100046, -104.7252558612402140, -7.842177630015021883 ) ) ;
#10450 = ORIENTED_EDGE ( 'NONE', *, *, #9333, .F. ) ;
#10451 = DIRECTION ( 'NONE',  ( -8.018662683283438208E-16, 5.975035461963189015E-16, 1.000000000000000000 ) ) ;
#10452 =( BOUNDED_CURVE ( )  B_SPLINE_CURVE ( 3, ( #2218, #8014, #7009, #8247 ),
 .UNSPECIFIED., .F., .T. ) 
 B_SPLINE_CURVE_WITH_KNOTS ( ( 4, 4 ),
 ( 1.628044839356179940, 3.141592653589792672 ),
 .UNSPECIFIED. ) 
 CURVE ( )  GEOMETRIC_REPRESENTATION_ITEM ( )  RATIONAL_B_SPLINE_CURVE ( ( 1.000000000000000000, 0.8180365063541270576, 0.8180365063541270576, 1.000000000000000000 ) ) 
 REPRESENTATION_ITEM ( '' )  );
#10453 = CARTESIAN_POINT ( 'NONE',  ( -25.24719169991952583, -11.38911842147176756, 57.00231026484397745 ) ) ;
#10454 = VECTOR ( 'NONE', #3937, 1000.000000000000000 ) ;
#10455 = CONTEXT_DEPENDENT_SHAPE_REPRESENTATION ( #13883, #1634 ) ;
#10456 = DIRECTION ( 'NONE',  ( 1.000000000000000000, 1.201369187114119994E-15, 9.616040805000176517E-16 ) ) ;
#10457 = VECTOR ( 'NONE', #13259, 1000.000000000000114 ) ;
#10458 = DIRECTION ( 'NONE',  ( -8.018662683283438208E-16, 5.975035461963189015E-16, 1.000000000000000000 ) ) ;
#10459 = EDGE_CURVE ( 'NONE', #5847, #964, #10024, .T. ) ;
#10460 = CARTESIAN_POINT ( 'NONE',  ( -15.49969986081099904, -36.50737899243799944, -13.49768973515600479 ) ) ;
#10461 = ORIENTED_EDGE ( 'NONE', *, *, #13256, .T. ) ;
#10462 = CARTESIAN_POINT ( 'NONE',  ( -10.02446058099324588, -7.572113216692248017, 56.85231026484398598 ) ) ;
#10463 = EDGE_CURVE ( 'NONE', #14564, #4445, #10310, .T. ) ;
#10464 = LINE ( 'NONE', #8159, #11191 ) ;
#10465 = PLANE ( 'NONE',  #4008 ) ;
#10466 = EDGE_CURVE ( 'NONE', #7470, #1944, #3998, .T. ) ;
#10467 = CARTESIAN_POINT ( 'NONE',  ( -38.20013690429809827, 4.873818854045000037, 27.91208557747711083 ) ) ;
#10468 = ORIENTED_EDGE ( 'NONE', *, *, #6382, .T. ) ;
#10469 = DIRECTION ( 'NONE',  ( 8.018662683283438208E-16, -5.975035461963189015E-16, -1.000000000000000000 ) ) ;
#10470 = ORIENTED_EDGE ( 'NONE', *, *, #13105, .T. ) ;
#10471 = LINE ( 'NONE', #2214, #6878 ) ;
#10472 = CARTESIAN_POINT ( 'NONE',  ( 2.500300139189001403, -46.50737899243799944, -2.497689735156001678 ) ) ;
#10473 = EDGE_CURVE ( 'NONE', #8967, #14193, #3147, .T. ) ;
#10474 = DIRECTION ( 'NONE',  ( 1.000000000000000000, -1.291538348938060198E-32, 1.054621095516909827E-16 ) ) ;
#10475 =( NAMED_UNIT ( * ) PLANE_ANGLE_UNIT ( ) SI_UNIT ( $, .RADIAN. ) );
#10476 = CYLINDRICAL_SURFACE ( 'NONE', #6493, 37.50000000000000000 ) ;
#10477 = LINE ( 'NONE', #3516, #12372 ) ;
#10478 = EDGE_CURVE ( 'NONE', #5664, #10716, #9835, .T. ) ;
#10479 = CARTESIAN_POINT ( 'NONE',  ( -13.16883223745437448, -21.23902216335526916, 57.00231026484399166 ) ) ;
#10480 = ADVANCED_FACE ( 'NONE', ( #6033 ), #10793, .F. ) ;
#10481 = CARTESIAN_POINT ( 'NONE',  ( -7.902754534677060683, -18.47202114588016642, 56.85231026484400019 ) ) ;
#10482 = CYLINDRICAL_SURFACE ( 'NONE', #5447, 1.249999999999999778 ) ;
#10483 = ORIENTED_EDGE ( 'NONE', *, *, #11827, .F. ) ;
#10484 = DIRECTION ( 'NONE',  ( -8.018662683283438208E-16, 5.975035461963189015E-16, 1.000000000000000000 ) ) ;
#10485 = PRODUCT_DEFINITION_CONTEXT ( 'detailed design', #4297, 'design' ) ;
#10486 = CIRCLE ( 'NONE', #9760, 2.500000000000000444 ) ;
#10487 = ORIENTED_EDGE ( 'NONE', *, *, #14124, .F. ) ;
#10489 = ORIENTED_EDGE ( 'NONE', *, *, #14148, .T. ) ;
#10488 = CARTESIAN_POINT ( 'NONE',  ( -8.569834614884436874, -19.36726104528708703, 56.85231026484400019 ) ) ;
#10490 = ORIENTED_EDGE ( 'NONE', *, *, #8604, .T. ) ;
#10491 = FACE_OUTER_BOUND ( 'NONE', #12735, .T. ) ;
#10492 = ORIENTED_EDGE ( 'NONE', *, *, #1118, .T. ) ;
#10493 = CARTESIAN_POINT ( 'NONE',  ( -18.61476135779618346, -20.95734656753543845, 56.85231026484398598 ) ) ;
#10494 = PLANE ( 'NONE',  #2817 ) ;
#10495 = DIRECTION ( 'NONE',  ( 0.000000000000000000, -1.000000000000000000, -1.224646799147350002E-16 ) ) ;
#10496 = DIRECTION ( 'NONE',  ( 0.8018662683283436232, -0.5975035461963189576, 9.999999999999996833E-16 ) ) ;
#10497 = VECTOR ( 'NONE', #14053, 1000.000000000000000 ) ;
#10498 = CARTESIAN_POINT ( 'NONE',  ( -11.97987666612771207, -20.77526002325937782, 56.85231026484400019 ) ) ;
#10499 = CARTESIAN_POINT ( 'NONE',  ( -23.08997828711216371, -47.08833727929018664, -17.22206101019868996 ) ) ;
#10500 = ORIENTED_EDGE ( 'NONE', *, *, #73, .F. ) ;
#10501 = EDGE_CURVE ( 'NONE', #13375, #8329, #10944, .T. ) ;
#10502 = CARTESIAN_POINT ( 'NONE',  ( 3.378223036541276425, -39.17044586890330038, -12.89965965032132011 ) ) ;
#10503 = EDGE_LOOP ( 'NONE', ( #3804, #11205 ) ) ;
#10504 = PLANE ( 'NONE',  #14590 ) ;
#10505 = VERTEX_POINT ( 'NONE', #9647 ) ;
#10506 = ORIENTED_EDGE ( 'NONE', *, *, #11461, .T. ) ;
#10507 = CARTESIAN_POINT ( 'NONE',  ( 3.575068303653157198, -38.90440891069084728, 51.78879027551830916 ) ) ;
#10508 = ORIENTED_EDGE ( 'NONE', *, *, #5408, .F. ) ;
#10509 = DIRECTION ( 'NONE',  ( 0.6251242923673534513, 0.7805252200231685977, 3.489949670250099574E-17 ) ) ;
#10510 = EDGE_CURVE ( 'NONE', #14042, #4372, #9163, .T. ) ;
#10511 = ADVANCED_FACE ( 'NONE', ( #1910 ), #9312, .T. ) ;
#10512 = CARTESIAN_POINT ( 'NONE',  ( -11.62590802060972628, -90.89463901465936146, -9.231817515786266526 ) ) ;
#10513 = VECTOR ( 'NONE', #14632, 1000.000000000000000 ) ;
#10514 = CARTESIAN_POINT ( 'NONE',  ( -7.519596205739571104, -45.08052302622432705, 21.55821474351395750 ) ) ;
#10516 = CARTESIAN_POINT ( 'NONE',  ( -2.216578225681298697, -31.14135358865360104, 59.46602571891969546 ) ) ;
#10515 = FACE_OUTER_BOUND ( 'NONE', #8729, .T. ) ;
#10517 = ORIENTED_EDGE ( 'NONE', *, *, #3367, .T. ) ;
#10518 = DIRECTION ( 'NONE',  ( 8.018662683283438208E-16, -5.975035461963189015E-16, -1.000000000000000000 ) ) ;
#10519 = CARTESIAN_POINT ( 'NONE',  ( -15.49969986081099904, -27.00737899243800300, -13.49768973515600301 ) ) ;
#10520 = ORIENTED_EDGE ( 'NONE', *, *, #8872, .F. ) ;
#10521 = ORIENTED_EDGE ( 'NONE', *, *, #1583, .T. ) ;
#10522 = CARTESIAN_POINT ( 'NONE',  ( -20.87112600995945755, -109.5609729487397885, -2.351181146270280298 ) ) ;
#10523 = DIRECTION ( 'NONE',  ( 0.5975035461963189576, 0.8018662683283437342, 0.000000000000000000 ) ) ;
#10524 = EDGE_LOOP ( 'NONE', ( #13465, #3994, #70, #5031 ) ) ;
#10525 = CARTESIAN_POINT ( 'NONE',  ( -7.499699860810999041, -43.97742925780038092, -17.13441993860075385 ) ) ;
#10526 = EDGE_LOOP ( 'NONE', ( #5958, #1851, #1941, #2756 ) ) ;
#10527 = EDGE_CURVE ( 'NONE', #15014, #7674, #598, .T. ) ;
#10528 = CARTESIAN_POINT ( 'NONE',  ( -20.36203582816999713, -107.1622034095870077, -6.087689735156004645 ) ) ;
#10529 = CARTESIAN_POINT ( 'NONE',  ( -12.85501980268021072, -23.15896895518548959, 56.90921755714956021 ) ) ;
#10530 = CARTESIAN_POINT ( 'NONE',  ( -31.79969986081099975, 3.992621007561997892, 24.26206422150100650 ) ) ;
#10531 = CARTESIAN_POINT ( 'NONE',  ( -10.90377457632059865, -6.867868786151726468, 56.85231026484398598 ) ) ;
#10532 = ORIENTED_EDGE ( 'NONE', *, *, #1737, .T. ) ;
#10533 = CARTESIAN_POINT ( 'NONE',  ( -3.499699860810999041, -57.00737899243800655, 52.39987856403599409 ) ) ;
#10534 = CYLINDRICAL_SURFACE ( 'NONE', #7494, 3.000000000000000000 ) ;
#10535 = VERTEX_POINT ( 'NONE', #6241 ) ;
#10536 = CARTESIAN_POINT ( 'NONE',  ( -18.09969986081100402, -102.1254310020070761, -6.517500700007478720 ) ) ;
#10537 = ORIENTED_EDGE ( 'NONE', *, *, #7255, .F. ) ;
#10538 = CARTESIAN_POINT ( 'NONE',  ( 13.85920135429429934, -27.00737899243800300, 24.21206422150099868 ) ) ;
#10539 = VERTEX_POINT ( 'NONE', #11075 ) ;
#10540 = AXIS2_PLACEMENT_3D ( 'NONE', #12119, #13643, #4078 ) ;
#10541 = DIRECTION ( 'NONE',  ( 3.839882694219489529E-17, -1.000000000000000000, 0.000000000000000000 ) ) ;
#10542 = FACE_BOUND ( 'NONE', #9309, .T. ) ;
#10543 = EDGE_CURVE ( 'NONE', #12074, #10009, #4452, .T. ) ;
#10544 = CARTESIAN_POINT ( 'NONE',  ( -21.12809094326923187, -9.219901432974651811, 56.85231026484398598 ) ) ;
#10545 = SURFACE_STYLE_USAGE ( .BOTH. , #1217 ) ;
#10546 = EDGE_CURVE ( 'NONE', #532, #7892, #8768, .T. ) ;
#10547 = LINE ( 'NONE', #8322, #902 ) ;
#10548 = CIRCLE ( 'NONE', #5175, 23.00000000000000000 ) ;
#10549 = VECTOR ( 'NONE', #1547, 1000.000000000000000 ) ;
#10550 = FACE_BOUND ( 'NONE', #487, .T. ) ;
#10551 = CARTESIAN_POINT ( 'NONE',  ( -15.54961651457173488, -13.51026476396819831, 56.85231026484398598 ) ) ;
#10552 = DIRECTION ( 'NONE',  ( -8.018662683283438208E-16, 5.975035461963189015E-16, 1.000000000000000000 ) ) ;
#10553 = DIRECTION ( 'NONE',  ( -0.9755678736739583634, 0.2196982563774038943, -9.135454576426008610E-16 ) ) ;
#10554 = ORIENTED_EDGE ( 'NONE', *, *, #6887, .F. ) ;
#10555 = CARTESIAN_POINT ( 'NONE',  ( -15.61203582817000068, -107.8163049764641812, -5.262754992868533321 ) ) ;
#10556 = EDGE_LOOP ( 'NONE', ( #11296, #10134, #11258, #9416 ) ) ;
#10557 = EDGE_CURVE ( 'NONE', #13947, #7202, #7044, .T. ) ;
#10559 = VERTEX_POINT ( 'NONE', #7397 ) ;
#10558 = LINE ( 'NONE', #5880, #13291 ) ;
#10560 = EDGE_LOOP ( 'NONE', ( #11560, #12462, #9178, #7779, #12485, #12559 ) ) ;
#10561 = CIRCLE ( 'NONE', #789, 9.974999999999999645 ) ;
#10562 = CARTESIAN_POINT ( 'NONE',  ( -37.04494295528539993, 20.99262100756200056, 32.26206422150099939 ) ) ;
#10563 = EDGE_LOOP ( 'NONE', ( #311, #12224 ) ) ;
#10564 = AXIS2_PLACEMENT_3D ( 'NONE', #8524, #14195, #11821 ) ;
#10565 = DIRECTION ( 'NONE',  ( -8.018662683283438208E-16, 5.975035461963189015E-16, 1.000000000000000000 ) ) ;
#10566 = EDGE_CURVE ( 'NONE', #9137, #8638, #14227, .T. ) ;
#10567 = EDGE_CURVE ( 'NONE', #2754, #9043, #4112, .T. ) ;
#10568 = DIRECTION ( 'NONE',  ( 0.9999272109403024578, -0.01206535623791937274, 8.090169943749475688E-16 ) ) ;
#10569 = EDGE_CURVE ( 'NONE', #14718, #5530, #5041, .T. ) ;
#10570 = CARTESIAN_POINT ( 'NONE',  ( 0.5796456139481135361, -52.92803351767889097, -14.44614973369544586 ) ) ;
#10571 = CARTESIAN_POINT ( 'NONE',  ( 18.10089137489735123, -24.75016685675518247, 7.560273441128909866 ) ) ;
#10572 = CARTESIAN_POINT ( 'NONE',  ( -12.51218212982932165, -9.498047650796509700, 54.00231026484399166 ) ) ;
#10573 = AXIS2_PLACEMENT_3D ( 'NONE', #8280, #11653, #14183 ) ;
#10574 = VECTOR ( 'NONE', #10165, 1000.000000000000000 ) ;
#10575 = CARTESIAN_POINT ( 'NONE',  ( -15.49969986081099904, 70.89785811302749607, 15.32568252027467004 ) ) ;
#10576 = EDGE_LOOP ( 'NONE', ( #10629, #11883, #11109, #11108 ) ) ;
#10577 = CARTESIAN_POINT ( 'NONE',  ( 2.884402102475247531, -40.07747304542361633, -13.18227376421650199 ) ) ;
#10578 = ORIENTED_EDGE ( 'NONE', *, *, #8586, .T. ) ;
#10579 = ORIENTED_EDGE ( 'NONE', *, *, #7090, .F. ) ;
#10580 = EDGE_LOOP ( 'NONE', ( #11201, #12128, #9824, #12238 ) ) ;
#10581 = CARTESIAN_POINT ( 'NONE',  ( 4.396918593460392266, -38.07367433586049543, 51.28992524861065050 ) ) ;
#10582 = VERTEX_POINT ( 'NONE', #12002 ) ;
#10583 = FACE_OUTER_BOUND ( 'NONE', #3028, .T. ) ;
#10584 = EDGE_CURVE ( 'NONE', #9118, #8928, #13267, .T. ) ;
#10585 = EDGE_CURVE ( 'NONE', #1699, #6007, #6638, .T. ) ;
#10586 = AXIS2_PLACEMENT_3D ( 'NONE', #3789, #6067, #10749 ) ;
#10587 = CARTESIAN_POINT ( 'NONE',  ( -15.49969986081091200, -13.50737899243823215, 48.00231026484398456 ) ) ;
#10588 = EDGE_CURVE ( 'NONE', #11595, #10638, #67, .T. ) ;
#10589 = CARTESIAN_POINT ( 'NONE',  ( -22.86200450971638531, -18.81376385001357932, 57.00231026484397745 ) ) ;
#10590 = AXIS2_PLACEMENT_3D ( 'NONE', #12444, #6604, #3182 ) ;
#10591 = CARTESIAN_POINT ( 'NONE',  ( -10.99969986081100082, -13.50737899243800122, 6.712064221500998684 ) ) ;
#10593 = CARTESIAN_POINT ( 'NONE',  ( -5.499699860811000818, -46.50737899243799944, 19.50231026484399877 ) ) ;
#10592 = CARTESIAN_POINT ( 'NONE',  ( -7.664252951136423242, -48.41696643141921896, -7.111243861656096676 ) ) ;
#10594 = ORIENTED_EDGE ( 'NONE', *, *, #9157, .T. ) ;
#10595 = CARTESIAN_POINT ( 'NONE',  ( -15.49969986081092088, -13.50737899243822504, 56.85231026484398598 ) ) ;
#10596 = CARTESIAN_POINT ( 'NONE',  ( -6.726903101582546007, -11.18374239837452500, 56.85231026484400019 ) ) ;
#10597 = ORIENTED_EDGE ( 'NONE', *, *, #8493, .T. ) ;
#10598 = ORIENTED_EDGE ( 'NONE', *, *, #6368, .F. ) ;
#10599 = CARTESIAN_POINT ( 'NONE',  ( 21.99138435360703525, -30.15310640139978915, 23.36840399548836444 ) ) ;
#10600 = EDGE_CURVE ( 'NONE', #14720, #1308, #3970, .T. ) ;
#10601 = VECTOR ( 'NONE', #4966, 1000.000000000000000 ) ;
#10602 = DIRECTION ( 'NONE',  ( 0.000000000000000000, 0.000000000000000000, -1.000000000000000000 ) ) ;
#10603 = ORIENTED_EDGE ( 'NONE', *, *, #14237, .F. ) ;
#10604 = CARTESIAN_POINT ( 'NONE',  ( -13.28079301173263005, -15.16077777396758464, 51.00231026484399166 ) ) ;
#10605 = EDGE_LOOP ( 'NONE', ( #11774, #8748, #7390, #2457, #12644 ) ) ;
#10606 = DIRECTION ( 'NONE',  ( -0.9316361277244822325, -0.3633925226508277206, -5.299192642332030163E-16 ) ) ;
#10607 = AXIS2_PLACEMENT_3D ( 'NONE', #5024, #2928, #9682 ) ;
#10608 = DIRECTION ( 'NONE',  ( -0.08178736187251967049, -0.9966498018049938512, 5.299192642332050870E-16 ) ) ;
#10609 = DIRECTION ( 'NONE',  ( 0.5975035461963189576, 0.8018662683283437342, 0.000000000000000000 ) ) ;
#10610 = CARTESIAN_POINT ( 'NONE',  ( -18.48721759179250412, -17.51671033407995282, 45.50231026484398456 ) ) ;
#10611 = ORIENTED_EDGE ( 'NONE', *, *, #2164, .F. ) ;
#10612 = CARTESIAN_POINT ( 'NONE',  ( -15.49969986081099904, -13.50737899243800122, 6.712064221500998684 ) ) ;
#10613 = FACE_OUTER_BOUND ( 'NONE', #8954, .T. ) ;
#10614 = CONICAL_SURFACE ( 'NONE', #5967, 15.87500000000000355, 0.1448623279155291654 ) ;
#10615 = EDGE_LOOP ( 'NONE', ( #4200, #4162, #3756, #4728 ) ) ;
#10616 = EDGE_CURVE ( 'NONE', #11595, #2901, #2816, .T. ) ;
#10617 = LINE ( 'NONE', #14291, #2428 ) ;
#10618 = ORIENTED_EDGE ( 'NONE', *, *, #6247, .T. ) ;
#10619 = PLANE ( 'NONE',  #4987 ) ;
#10620 = EDGE_LOOP ( 'NONE', ( #146, #6102 ) ) ;
#10621 = CARTESIAN_POINT ( 'NONE',  ( -15.49969986081099904, 20.99262100756200056, 24.21206422150100224 ) ) ;
#10622 = DIRECTION ( 'NONE',  ( 0.000000000000000000, 0.000000000000000000, 1.000000000000000000 ) ) ;
#10623 = CARTESIAN_POINT ( 'NONE',  ( -15.49969986081100437, -101.0987031166763188, -6.239619411973396090 ) ) ;
#10624 = LINE ( 'NONE', #11928, #7861 ) ;
#10625 = LINE ( 'NONE', #7169, #6938 ) ;
#10626 = CARTESIAN_POINT ( 'NONE',  ( -23.49969986081099904, -19.50737899243800300, 6.712064221500998684 ) ) ;
#10627 = CONICAL_SURFACE ( 'NONE', #5493, 1.769239858347549932, 0.8464846872172493430 ) ;
#10628 = DIRECTION ( 'NONE',  ( -8.018662683283438208E-16, 5.975035461963189015E-16, 1.000000000000000000 ) ) ;
#10629 = ORIENTED_EDGE ( 'NONE', *, *, #115, .T. ) ;
#10630 = CARTESIAN_POINT ( 'NONE',  ( -17.12834591918736749, -6.622385381944812188, 56.85231026484398598 ) ) ;
#10631 = CARTESIAN_POINT ( 'NONE',  ( -20.72181259498818306, -108.0168781946340033, -6.766942245938937894 ) ) ;
#10632 = DIRECTION ( 'NONE',  ( 8.018662683283438208E-16, -5.975035461963189015E-16, -1.000000000000000000 ) ) ;
#10633 = EDGE_CURVE ( 'NONE', #6219, #5382, #6879, .T. ) ;
#10634 = ORIENTED_EDGE ( 'NONE', *, *, #5649, .F. ) ;
#10635 = CARTESIAN_POINT ( 'NONE',  ( -8.162984683111186968, -16.88054299694650595, 57.00231026484399166 ) ) ;
#10636 = ORIENTED_EDGE ( 'NONE', *, *, #14341, .T. ) ;
#10638 = VERTEX_POINT ( 'NONE', #8695 ) ;
#10637 = DIRECTION ( 'NONE',  ( 0.000000000000000000, -1.000000000000000000, -1.224646799147350002E-16 ) ) ;
#10639 = VERTEX_POINT ( 'NONE', #13377 ) ;
#10640 = EDGE_CURVE ( 'NONE', #14240, #34, #11057, .T. ) ;
#10641 = CARTESIAN_POINT ( 'NONE',  ( -31.79969986081099975, 20.99262100756200056, 24.21206422150100224 ) ) ;
#10642 = ORIENTED_EDGE ( 'NONE', *, *, #14642, .F. ) ;
#10643 = CARTESIAN_POINT ( 'NONE',  ( -5.499699860810999041, -19.50737899243799589, -123.9247733198440073 ) ) ;
#10644 = CARTESIAN_POINT ( 'NONE',  ( -15.49969986081099904, -32.00737899243799944, 19.50231026484400232 ) ) ;
#10645 = CARTESIAN_POINT ( 'NONE',  ( 18.53245405280430802, -27.00737899243800300, 8.462064221501000461 ) ) ;
#10646 = CARTESIAN_POINT ( 'NONE',  ( -15.49969986081092088, -13.50737899243822504, 56.85231026484398598 ) ) ;
#10647 = CARTESIAN_POINT ( 'NONE',  ( -6.766506000727597225, -11.03906478995046214, 56.85231026484400019 ) ) ;
#10648 = EDGE_CURVE ( 'NONE', #818, #7911, #7768, .T. ) ;
#10649 = VECTOR ( 'NONE', #129, 1000.000000000000000 ) ;
#10650 = CARTESIAN_POINT ( 'NONE',  ( 3.680269495751442577, -38.76197583039466110, -12.72242068341919286 ) ) ;
#10651 = ADVANCED_FACE ( 'NONE', ( #13747 ), #3036, .F. ) ;
#10652 = ORIENTED_EDGE ( 'NONE', *, *, #14224, .T. ) ;
#10653 = VECTOR ( 'NONE', #6849, 1000.000000000000227 ) ;
#10654 = ORIENTED_EDGE ( 'NONE', *, *, #8124, .T. ) ;
#10655 = EDGE_LOOP ( 'NONE', ( #511, #1241, #4582, #1730, #8388 ) ) ;
#10656 = EDGE_CURVE ( 'NONE', #10870, #5903, #11789, .T. ) ;
#10657 = CARTESIAN_POINT ( 'NONE',  ( -21.68801466096620700, -19.44379288755867208, 56.85231026484398598 ) ) ;
#10658 = ORIENTED_EDGE ( 'NONE', *, *, #6951, .F. ) ;
#10659 = CARTESIAN_POINT ( 'NONE',  ( -18.51905911803493865, -23.07164644789430596, 56.88620726433236285 ) ) ;
#10660 = EDGE_CURVE ( 'NONE', #9137, #7024, #898, .T. ) ;
#10661 = B_SPLINE_CURVE_WITH_KNOTS ( 'NONE', 3,
 ( #13510, #10046, #7530, #14577 ),
 .UNSPECIFIED., .F., .F.,
 ( 4, 4 ),
 ( 0.01169941957287599921, 0.01381006638855979997 ),
 .UNSPECIFIED. ) ;
#10662 =( NAMED_UNIT ( * ) PLANE_ANGLE_UNIT ( ) SI_UNIT ( $, .RADIAN. ) );
#10663 = CARTESIAN_POINT ( 'NONE',  ( -24.53816276005083452, -12.69040994830970703, 56.85231026484398598 ) ) ;
#10664 = PLANE ( 'NONE',  #8655 ) ;
#10666 = DIRECTION ( 'NONE',  ( 1.000000000000000000, 1.201369187114119994E-15, 9.616040805000176517E-16 ) ) ;
#10665 = LINE ( 'NONE', #2636, #522 ) ;
#10667 = ORIENTED_EDGE ( 'NONE', *, *, #8757, .T. ) ;
#10668 = CARTESIAN_POINT ( 'NONE',  ( -15.19697172008446096, -10.92700001391350284, 51.00231026484399166 ) ) ;
#10669 = EDGE_CURVE ( 'NONE', #13407, #4277, #13748, .T. ) ;
#10670 = CARTESIAN_POINT ( 'NONE',  ( -20.18599136182623965, -36.50737899243796392, 2.502310264844031629 ) ) ;
#10671 = ORIENTED_EDGE ( 'NONE', *, *, #1369, .F. ) ;
#10672 = ORIENTED_EDGE ( 'NONE', *, *, #3385, .F. ) ;
#10673 = LINE ( 'NONE', #12984, #7121 ) ;
#10674 = CARTESIAN_POINT ( 'NONE',  ( -16.02964405221278099, -52.50737899243799944, 57.00231026484399166 ) ) ;
#10675 = VECTOR ( 'NONE', #13457, 1000.000000000000000 ) ;
#10676 = ORIENTED_EDGE ( 'NONE', *, *, #7093, .T. ) ;
#10677 = VECTOR ( 'NONE', #6738, 1000.000000000000000 ) ;
#10678 = DIRECTION ( 'NONE',  ( 0.3633925226508277206, -0.9316361277244822325, 8.480480961564270869E-16 ) ) ;
#10679 = AXIS2_PLACEMENT_3D ( 'NONE', #8618, #2731, #7157 ) ;
#10680 = PRODUCT_DEFINITION ( 'UNKNOWN', '', #6801, #10485 ) ;
#10681 = EDGE_CURVE ( 'NONE', #12259, #8545, #6397, .T. ) ;
#10682 = VECTOR ( 'NONE', #7460, 1000.000000000000000 ) ;
#10683 = FACE_OUTER_BOUND ( 'NONE', #2994, .T. ) ;
#10684 = CARTESIAN_POINT ( 'NONE',  ( 22.00030013918900096, -27.00737899243800300, 40.71206422150099513 ) ) ;
#10685 = AXIS2_PLACEMENT_3D ( 'NONE', #1232, #2387, #14167 ) ;
#10686 = ORIENTED_EDGE ( 'NONE', *, *, #14971, .F. ) ;
#10687 = CARTESIAN_POINT ( 'NONE',  ( 4.000300139189000959, -20.37340439622240851, 51.53354502093799994 ) ) ;
#10688 = CARTESIAN_POINT ( 'NONE',  ( 9.000300139189000959, -27.00737899243800300, 24.21206422150099868 ) ) ;
#10689 = ORIENTED_EDGE ( 'NONE', *, *, #55, .T. ) ;
#10690 = DIRECTION ( 'NONE',  ( 0.1272150336605032961, -0.9918751611018177261, 6.946583704589934213E-16 ) ) ;
#10691 = CARTESIAN_POINT ( 'NONE',  ( -17.54662770128649285, -5.179934221328323929, 56.85231026484398598 ) ) ;
#10692 = ORIENTED_EDGE ( 'NONE', *, *, #11672, .F. ) ;
#10693 = DIRECTION ( 'NONE',  ( 8.018662683283438208E-16, -5.975035461963189015E-16, -1.000000000000000000 ) ) ;
#10694 = ORIENTED_EDGE ( 'NONE', *, *, #656, .T. ) ;
#10695 = DIRECTION ( 'NONE',  ( 1.000000000000000000, -1.291538348938060198E-32, 1.054621095516909827E-16 ) ) ;
#10696 = CARTESIAN_POINT ( 'NONE',  ( -18.09969986081100402, -109.0157871265392799, -1.700811998197179431 ) ) ;
#10697 = AXIS2_PLACEMENT_3D ( 'NONE', #6100, #3976, #12011 ) ;
#10698 = VECTOR ( 'NONE', #2565, 1000.000000000000000 ) ;
#10699 = AXIS2_PLACEMENT_3D ( 'NONE', #5743, #7184, #11786 ) ;
#10700 = LINE ( 'NONE', #8397, #2493 ) ;
#10701 = EDGE_CURVE ( 'NONE', #150, #5925, #6465, .T. ) ;
#10702 = ADVANCED_FACE ( 'NONE', ( #5551 ), #3192, .F. ) ;
#10703 = CARTESIAN_POINT ( 'NONE',  ( -6.891327302372677543, -18.62408673770649159, 60.71152943577731520 ) ) ;
#10704 = LINE ( 'NONE', #8403, #4302 ) ;
#10705 = VERTEX_POINT ( 'NONE', #11297 ) ;
#10706 = DIRECTION ( 'NONE',  ( 1.000000000000000000, 1.201369187114119994E-15, 9.616040805000176517E-16 ) ) ;
#10707 = VECTOR ( 'NONE', #14414, 1000.000000000000000 ) ;
#10708 = CARTESIAN_POINT ( 'NONE',  ( -33.88380182411292196, -40.07747304539473276, 52.18689429389564083 ) ) ;
#10709 = DIRECTION ( 'NONE',  ( -1.000000000000000000, -1.201369187114119994E-15, -9.616040805000176517E-16 ) ) ;
#10710 = VECTOR ( 'NONE', #12471, 1000.000000000000000 ) ;
#10711 = ORIENTED_EDGE ( 'NONE', *, *, #4092, .T. ) ;
#10712 = CARTESIAN_POINT ( 'NONE',  ( 7.361522891262090695, 4.383170266556664529, 21.67185847294893719 ) ) ;
#10713 = ORIENTED_EDGE ( 'NONE', *, *, #2531, .F. ) ;
#10715 = ORIENTED_EDGE ( 'NONE', *, *, #8063, .T. ) ;
#10714 = CARTESIAN_POINT ( 'NONE',  ( -17.91037007046713470, -11.71108944158557463, 57.00231026484397745 ) ) ;
#10716 = VERTEX_POINT ( 'NONE', #12606 ) ;
#10717 = CARTESIAN_POINT ( 'NONE',  ( -14.00164528647249007, -5.572553380472728968, 56.85231026484398598 ) ) ;
#10718 = LINE ( 'NONE', #5884, #927 ) ;
#10719 = ORIENTED_EDGE ( 'NONE', *, *, #14499, .T. ) ;
#10720 = DIRECTION ( 'NONE',  ( 0.000000000000000000, 1.000000000000000000, 0.000000000000000000 ) ) ;
#10721 = CARTESIAN_POINT ( 'NONE',  ( -34.24293707257970709, 11.48902252484896991, 16.16206422150067823 ) ) ;
#10722 = VECTOR ( 'NONE', #660, 1000.000000000000000 ) ;
#10723 = ADVANCED_FACE ( 'NONE', ( #11447 ), #2119, .T. ) ;
#10724 = AXIS2_PLACEMENT_3D ( 'NONE', #8212, #2483, #4632 ) ;
#10725 = CARTESIAN_POINT ( 'NONE',  ( -3.499699860810999041, -57.00737899243800655, -16.02584758213710003 ) ) ;
#10726 = DIRECTION ( 'NONE',  ( 1.000000000000000000, 1.160894772049054314E-15, -9.869715661189392962E-16 ) ) ;
#10727 = CARTESIAN_POINT ( 'NONE',  ( -15.49969986081092088, -13.50737899243822504, 57.00231026484397745 ) ) ;
#10728 = VECTOR ( 'NONE', #8430, 1000.000000000000114 ) ;
#10729 = LINE ( 'NONE', #106, #5438 ) ;
#10730 = LINE ( 'NONE', #408, #13255 ) ;
#10731 = VERTEX_POINT ( 'NONE', #667 ) ;
#10732 = ORIENTED_EDGE ( 'NONE', *, *, #1951, .F. ) ;
#10733 = ORIENTED_EDGE ( 'NONE', *, *, #9814, .F. ) ;
#10734 = CARTESIAN_POINT ( 'NONE',  ( 3.273611621580635678, -39.31333522019950522, 51.96562901102289800 ) ) ;
#10735 = ORIENTED_EDGE ( 'NONE', *, *, #11443, .F. ) ;
#10736 = CARTESIAN_POINT ( 'NONE',  ( -23.54764701038621411, -12.84694604531765272, 56.85231026484398598 ) ) ;
#10737 = CARTESIAN_POINT ( 'NONE',  ( -15.49969986081099904, 64.39262100756199914, 18.96206422150100579 ) ) ;
#10738 = VECTOR ( 'NONE', #6655, 1000.000000000000000 ) ;
#10739 = CIRCLE ( 'NONE', #5843, 0.2000000000000012046 ) ;
#10740 = ADVANCED_FACE ( 'NONE', ( #6692 ), #5333, .F. ) ;
#10741 = DIRECTION ( 'NONE',  ( 0.5975035461963189576, 0.8018662683283437342, 0.000000000000000000 ) ) ;
#10742 = CARTESIAN_POINT ( 'NONE',  ( -17.72286745096105065, -3.783277446994219417, 57.00231026484397745 ) ) ;
#10743 = EDGE_CURVE ( 'NONE', #3090, #2245, #6541, .T. ) ;
#10744 = DIRECTION ( 'NONE',  ( 0.000000000000000000, 1.224646799147350002E-16, -1.000000000000000000 ) ) ;
#10746 = CARTESIAN_POINT ( 'NONE',  ( -15.61203582817000068, -106.7748397497402806, -5.108753790441425302 ) ) ;
#10745 = CARTESIAN_POINT ( 'NONE',  ( -7.611722567307242393, -48.62974432432520189, -4.173814398520391045 ) ) ;
#10747 = VERTEX_POINT ( 'NONE', #2959 ) ;
#10748 = CARTESIAN_POINT ( 'NONE',  ( -8.639554752241616953, -9.247137322136806503, 56.85231026484400019 ) ) ;
#10749 = DIRECTION ( 'NONE',  ( -8.673617379884027583E-16, 1.000000000000000000, 0.000000000000000000 ) ) ;
#10750 = VERTEX_POINT ( 'NONE', #7618 ) ;
#10751 = ADVANCED_FACE ( 'NONE', ( #14744 ), #8840, .T. ) ;
#10752 = CIRCLE ( 'NONE', #4154, 9.974999999999999645 ) ;
#10753 = VERTEX_POINT ( 'NONE', #1894 ) ;
#10754 = CARTESIAN_POINT ( 'NONE',  ( 21.98610757316710718, -30.09037826958212491, 23.16186116307340725 ) ) ;
#10755 = CARTESIAN_POINT ( 'NONE',  ( -18.80568317180454940, -37.21776555879632298, 56.85708068924256509 ) ) ;
#10756 = CARTESIAN_POINT ( 'NONE',  ( -7.145558396657058609, -18.95797028117975103, 56.85231026484400019 ) ) ;
#10757 = VERTEX_POINT ( 'NONE', #11226 ) ;
#10758 = CARTESIAN_POINT ( 'NONE',  ( -13.42625477939331624, -36.76308351228195193, -17.94383996831232864 ) ) ;
#10759 = APPLICATION_CONTEXT ( 'automotive_design' ) ;
#10760 = MECHANICAL_DESIGN_GEOMETRIC_PRESENTATION_REPRESENTATION (  '', ( #741 ), #6096 ) ;
#10761 = EDGE_CURVE ( 'NONE', #9327, #6873, #4344, .T. ) ;
#10762 = CARTESIAN_POINT ( 'NONE',  ( -15.61203582816999891, -107.9196643519486969, -5.433976602192394090 ) ) ;
#10763 = ADVANCED_FACE ( 'NONE', ( #4263 ), #8994, .F. ) ;
#10764 = DIRECTION ( 'NONE',  ( -1.000000000000000000, 0.000000000000000000, 0.000000000000000000 ) ) ;
#10765 = DIRECTION ( 'NONE',  ( 1.000000000000000078E-15, -1.000000000000000000, 0.000000000000000000 ) ) ;
#10766 = FACE_OUTER_BOUND ( 'NONE', #13539, .T. ) ;
#10768 = VERTEX_POINT ( 'NONE', #10139 ) ;
#10767 = VECTOR ( 'NONE', #7261, 1000.000000000000000 ) ;
#10769 = CARTESIAN_POINT ( 'NONE',  ( -7.731023390221355207, -11.30308411758414877, 56.85231026484400019 ) ) ;
#10770 = SHAPE_REPRESENTATION ( 'Indexable Carbide Insert', ( #6789 ), #4119 ) ;
#10771 = DIRECTION ( 'NONE',  ( 1.000000000000000000, -3.922012711866029438E-32, 3.202566417187950042E-16 ) ) ;
#10772 = ORIENTED_EDGE ( 'NONE', *, *, #9701, .T. ) ;
#10773 = DIRECTION ( 'NONE',  ( 0.000000000000000000, 0.000000000000000000, 1.000000000000000000 ) ) ;
#10774 = FACE_OUTER_BOUND ( 'NONE', #5673, .T. ) ;
#10775 = VERTEX_POINT ( 'NONE', #14817 ) ;
#10776 = CARTESIAN_POINT ( 'NONE',  ( -37.04494295528539993, 12.99262100756199878, 16.16206422150100153 ) ) ;
#10777 = VERTEX_POINT ( 'NONE', #2628 ) ;
#10778 = FACE_OUTER_BOUND ( 'NONE', #14853, .T. ) ;
#10779 = CARTESIAN_POINT ( 'NONE',  ( -10.12827371166239843, -85.00737899243800655, -5.497689735155993240 ) ) ;
#10780 = EDGE_CURVE ( 'NONE', #633, #1609, #14202, .T. ) ;
#10781 = CARTESIAN_POINT ( 'NONE',  ( -33.49969986081099904, -42.00737899243800655, -13.39525803434800011 ) ) ;
#10782 = CARTESIAN_POINT ( 'NONE',  ( 15.62491684846984619, -29.63902260056506321, 3.294372889119066450 ) ) ;
#10783 = ORIENTED_EDGE ( 'NONE', *, *, #8675, .T. ) ;
#10784 = CARTESIAN_POINT ( 'NONE',  ( -14.61203582816999891, -108.2036686363109084, -6.241690937583107335 ) ) ;
#10785 = CARTESIAN_POINT ( 'NONE',  ( -15.49969986081091022, -13.50737899243823215, 45.50231026484398456 ) ) ;
#10786 = DIRECTION ( 'NONE',  ( 8.018662683283439195E-16, -5.975035461963190987E-16, -1.000000000000000000 ) ) ;
#10787 = VERTEX_POINT ( 'NONE', #12757 ) ;
#10788 = DIRECTION ( 'NONE',  ( 0.8222303661035904598, -0.5691548339926103539, 9.993908270190959005E-16 ) ) ;
#10789 = ORIENTED_EDGE ( 'NONE', *, *, #14575, .T. ) ;
#10791 = ORIENTED_EDGE ( 'NONE', *, *, #1880, .T. ) ;
#10790 = CARTESIAN_POINT ( 'NONE',  ( -23.59621936791820573, -19.33378413377806382, 57.00231026484397745 ) ) ;
#10792 = ORIENTED_EDGE ( 'NONE', *, *, #1065, .F. ) ;
#10793 = PLANE ( 'NONE',  #12037 ) ;
#10794 = EDGE_CURVE ( 'NONE', #6250, #2134, #10816, .T. ) ;
#10795 = PLANE ( 'NONE',  #13263 ) ;
#10796 = ORIENTED_EDGE ( 'NONE', *, *, #10030, .F. ) ;
#10797 = DIRECTION ( 'NONE',  ( -1.000000000000000000, 0.000000000000000000, 0.000000000000000000 ) ) ;
#10798 = FACE_OUTER_BOUND ( 'NONE', #11287, .T. ) ;
#10799 = VECTOR ( 'NONE', #8024, 1000.000000000000000 ) ;
#10800 = CARTESIAN_POINT ( 'NONE',  ( -12.46042140754850003, -23.00808483377100089, 54.00231026484399166 ) ) ;
#10801 = DIRECTION ( 'NONE',  ( 0.000000000000000000, 0.000000000000000000, 1.000000000000000000 ) ) ;
#10802 = CARTESIAN_POINT ( 'NONE',  ( 17.94083381668699673, -24.45944232969977250, 7.241130984151665118 ) ) ;
#10803 = CARTESIAN_POINT ( 'NONE',  ( -15.49969986081099194, -27.00737899243800300, 11.50231026484399877 ) ) ;
#10804 = CIRCLE ( 'NONE', #2979, 9.974999999999999645 ) ;
#10805 = DIRECTION ( 'NONE',  ( -0.04695496274984587576, -0.9988970074402868660, 5.591929034707467802E-16 ) ) ;
#10806 = VECTOR ( 'NONE', #8674, 1000.000000000000000 ) ;
#10807 = VERTEX_POINT ( 'NONE', #1048 ) ;
#10808 = FILL_AREA_STYLE ('',( #6121 ) ) ;
#10809 = EDGE_LOOP ( 'NONE', ( #9601, #9634, #8203, #5110 ) ) ;
#10810 = ORIENTED_EDGE ( 'NONE', *, *, #12328, .T. ) ;
#10811 = ADVANCED_FACE ( 'NONE', ( #11522 ), #8582, .T. ) ;
#10812 = AXIS2_PLACEMENT_3D ( 'NONE', #14147, #2669, #3669 ) ;
#10813 = CARTESIAN_POINT ( 'NONE',  ( -15.61203582816999713, -107.9994814593942607, -7.057848339359948042 ) ) ;
#10814 = VERTEX_POINT ( 'NONE', #5706 ) ;
#10815 = EDGE_CURVE ( 'NONE', #5023, #10505, #347, .T. ) ;
#10816 = LINE ( 'NONE', #9299, #6127 ) ;
#10817 = CARTESIAN_POINT ( 'NONE',  ( -21.23124220554638697, -20.54376104222092181, 56.85231026484398598 ) ) ;
#10818 = FILL_AREA_STYLE_COLOUR ( '', #1474 ) ;
#10819 = CARTESIAN_POINT ( 'NONE',  ( -10.74382054100576234, -90.63416536375187604, -7.998061603526264385 ) ) ;
#10820 = VECTOR ( 'NONE', #4931, 1000.000000000000000 ) ;
#10821 = AXIS2_PLACEMENT_3D ( 'NONE', #10647, #3839, #2544 ) ;
#10822 = CARTESIAN_POINT ( 'NONE',  ( -25.44713467170207366, -12.76632185356751847, 56.85231026484398598 ) ) ;
#10823 = CARTESIAN_POINT ( 'NONE',  ( -7.629407442448592924, -48.55937836029033150, -4.069029971051592476 ) ) ;
#10824 = ORIENTED_EDGE ( 'NONE', *, *, #1417, .T. ) ;
#10825 = DIRECTION ( 'NONE',  ( -8.018662683283438208E-16, 5.975035461963189015E-16, 1.000000000000000000 ) ) ;
#10826 = FACE_OUTER_BOUND ( 'NONE', #5075, .T. ) ;
#10827 = ORIENTED_EDGE ( 'NONE', *, *, #8823, .T. ) ;
#10828 = ORIENTED_EDGE ( 'NONE', *, *, #11305, .F. ) ;
#10829 = EDGE_CURVE ( 'NONE', #4184, #8556, #41, .T. ) ;
#10830 = DIRECTION ( 'NONE',  ( -5.000000000000000389E-16, 0.4999999999999998890, 0.8660254037844387076 ) ) ;
#10831 = ORIENTED_EDGE ( 'NONE', *, *, #14592, .T. ) ;
#10832 = CARTESIAN_POINT ( 'NONE',  ( -25.24719169991952228, -11.38911842147176934, 54.00231026484397745 ) ) ;
#10833 = VECTOR ( 'NONE', #9326, 1000.000000000000227 ) ;
#10834 = ADVANCED_FACE ( 'NONE', ( #5007 ), #10373, .F. ) ;
#10835 = VECTOR ( 'NONE', #9057, 1000.000000000000000 ) ;
#10836 = CARTESIAN_POINT ( 'NONE',  ( -18.43409448121630945, -5.984417261063049942, 56.85231026484398598 ) ) ;
#10837 = CARTESIAN_POINT ( 'NONE',  ( -11.72862643632814716, -22.77130243382190500, 56.81215603131989411 ) ) ;
#10838 = EDGE_CURVE ( 'NONE', #3312, #6835, #7280, .T. ) ;
#10839 = AXIS2_PLACEMENT_3D ( 'NONE', #5111, #9776, #12604 ) ;
#10840 = CARTESIAN_POINT ( 'NONE',  ( -10.96544185377836911, -6.825182173602284408, 56.85231026484398598 ) ) ;
#10841 = DIRECTION ( 'NONE',  ( 0.000000000000000000, 0.000000000000000000, -1.000000000000000000 ) ) ;
#10842 = EDGE_LOOP ( 'NONE', ( #12658, #7057, #11573, #14754 ) ) ;
#10843 = DIRECTION ( 'NONE',  ( -8.018662683283438208E-16, 5.975035461963189015E-16, 1.000000000000000000 ) ) ;
#10844 = CARTESIAN_POINT ( 'NONE',  ( -7.495514965259227225, -43.99345095228514424, -5.341653756843942169 ) ) ;
#10845 = VERTEX_POINT ( 'NONE', #263 ) ;
#10846 = EDGE_CURVE ( 'NONE', #11369, #560, #6054, .T. ) ;
#10848 = EDGE_CURVE ( 'NONE', #551, #2842, #15039, .T. ) ;
#10847 = CARTESIAN_POINT ( 'NONE',  ( -18.09969986081091875, -107.1622034095862972, -7.162689735156003934 ) ) ;
#10849 = DIRECTION ( 'NONE',  ( -8.018662683283438208E-16, 5.975035461963189015E-16, 1.000000000000000000 ) ) ;
#10850 = ORIENTED_EDGE ( 'NONE', *, *, #136, .F. ) ;
#10851 = DIRECTION ( 'NONE',  ( 8.018662683283438208E-16, -5.975035461963189015E-16, -1.000000000000000000 ) ) ;
#10852 = AXIS2_PLACEMENT_3D ( 'NONE', #1725, #10050, #2951 ) ;
#10853 = ORIENTED_EDGE ( 'NONE', *, *, #2051, .F. ) ;
#10854 = DIRECTION ( 'NONE',  ( 0.000000000000000000, 0.1872998510044759646, 0.9823027872370621028 ) ) ;
#10855 = EDGE_CURVE ( 'NONE', #14217, #8353, #12680, .T. ) ;
#10856 = VECTOR ( 'NONE', #7726, 1000.000000000000227 ) ;
#10857 = DIRECTION ( 'NONE',  ( 0.9320450512859433934, -0.1973458207444490908, -0.3038859151196102171 ) ) ;
#10858 = EDGE_CURVE ( 'NONE', #4089, #8967, #11599, .T. ) ;
#10859 = CARTESIAN_POINT ( 'NONE',  ( -7.526618194427099340, -48.92257192762229323, 18.84067492369451813 ) ) ;
#10860 = CIRCLE ( 'NONE', #4758, 5.371426149148541107 ) ;
#10861 = CARTESIAN_POINT ( 'NONE',  ( 16.55868115085372594, -30.23116488229778653, 4.755404724957913665 ) ) ;
#10862 = ORIENTED_EDGE ( 'NONE', *, *, #4775, .T. ) ;
#10863 = CARTESIAN_POINT ( 'NONE',  ( -10.61529477037414715, -50.86499734049451149, -17.68083815942426895 ) ) ;
#10864 = LINE ( 'NONE', #392, #14374 ) ;
#10865 = CIRCLE ( 'NONE', #1821, 1.769239858347549932 ) ;
#10866 = ORIENTED_EDGE ( 'NONE', *, *, #7187, .T. ) ;
#10867 = FACE_OUTER_BOUND ( 'NONE', #7968, .T. ) ;
#10868 = EDGE_CURVE ( 'NONE', #4941, #6874, #8359, .T. ) ;
#10869 = EDGE_CURVE ( 'NONE', #7124, #9677, #4930, .T. ) ;
#10870 = VERTEX_POINT ( 'NONE', #3417 ) ;
#10872 = ORIENTED_EDGE ( 'NONE', *, *, #6272, .F. ) ;
#10871 = LINE ( 'NONE', #2605, #9114 ) ;
#10873 = ORIENTED_EDGE ( 'NONE', *, *, #8963, .F. ) ;
#10874 = CARTESIAN_POINT ( 'NONE',  ( -15.36741682587554969, -22.58172476492607572, 57.00231026484399166 ) ) ;
#10875 = DIRECTION ( 'NONE',  ( 1.000000000000000000, 0.000000000000000000, 0.000000000000000000 ) ) ;
#10876 = DIRECTION ( 'NONE',  ( 0.000000000000000000, -1.508455196501571676E-16, 1.000000000000000000 ) ) ;
#10877 = VECTOR ( 'NONE', #5134, 999.9999999999998863 ) ;
#10878 = LINE ( 'NONE', #6486, #13127 ) ;
#10879 = DIRECTION ( 'NONE',  ( 1.000000000000000000, 0.000000000000000000, 0.000000000000000000 ) ) ;
#10880 = DIRECTION ( 'NONE',  ( -0.8772189822852964891, 0.4800904676395363335, -9.902680687415702019E-16 ) ) ;
#10881 = ADVANCED_FACE ( 'NONE', ( #3778 ), #7203, .F. ) ;
#10882 = CARTESIAN_POINT ( 'NONE',  ( -20.36203582816999713, -106.9280785958314510, -4.859811251109673158 ) ) ;
#10883 = ORIENTED_EDGE ( 'NONE', *, *, #1808, .T. ) ;
#10884 = EDGE_LOOP ( 'NONE', ( #10890, #5123, #3430, #7557 ) ) ;
#10885 = CARTESIAN_POINT ( 'NONE',  ( -15.49969986081099904, -2.007378992438000331, 24.21206422150100579 ) ) ;
#10886 = ORIENTED_EDGE ( 'NONE', *, *, #4839, .F. ) ;
#10887 = ORIENTED_EDGE ( 'NONE', *, *, #8035, .F. ) ;
#10888 = CARTESIAN_POINT ( 'NONE',  ( -13.02562488396841900, -21.19439421350821817, 56.85231026484400019 ) ) ;
#10889 = VERTEX_POINT ( 'NONE', #11964 ) ;
#10890 = ORIENTED_EDGE ( 'NONE', *, *, #6848, .T. ) ;
#10891 = CARTESIAN_POINT ( 'NONE',  ( -20.33437667196779586, -7.039214636791314206, 56.85231026484398598 ) ) ;
#10892 = DIRECTION ( 'NONE',  ( 0.000000000000000000, -2.185478394931410082E-16, 1.000000000000000000 ) ) ;
#10893 = DIRECTION ( 'NONE',  ( 1.054621095516909827E-16, 1.224646799147350002E-16, -1.000000000000000000 ) ) ;
#10894 = EDGE_CURVE ( 'NONE', #9624, #13913, #13642, .T. ) ;
#10895 = VECTOR ( 'NONE', #1595, 1000.000000000000000 ) ;
#10896 = CARTESIAN_POINT ( 'NONE',  ( -9.565488148413143321, -20.37370125056455095, 56.85231026484400019 ) ) ;
#10898 = CARTESIAN_POINT ( 'NONE',  ( -37.01777924068312586, 5.443421374451959949, 19.56527334556399111 ) ) ;
#10897 = DIRECTION ( 'NONE',  ( 0.7582332219680881780, -0.6519834208811539078, 9.975640502598240034E-16 ) ) ;
#10899 = ORIENTED_EDGE ( 'NONE', *, *, #14809, .F. ) ;
#10900 = CARTESIAN_POINT ( 'NONE',  ( -11.97987666612771207, -20.77526002325937782, 57.00231026484399166 ) ) ;
#10901 = CARTESIAN_POINT ( 'NONE',  ( -24.80291049273179027, -17.17778628407305774, 60.53990586317451061 ) ) ;
#10902 = ORIENTED_EDGE ( 'NONE', *, *, #562, .F. ) ;
#10903 = ORIENTED_EDGE ( 'NONE', *, *, #3749, .T. ) ;
#10904 = CARTESIAN_POINT ( 'NONE',  ( -22.70654572567255158, -20.40389968624656802, 56.85231026484398598 ) ) ;
#10905 = ORIENTED_EDGE ( 'NONE', *, *, #1799, .T. ) ;
#10906 = VECTOR ( 'NONE', #10399, 1000.000000000000000 ) ;
#10907 = CARTESIAN_POINT ( 'NONE',  ( -15.49969986081099904, 2.992621007561997004, 24.21206422150099868 ) ) ;
#10908 = EDGE_CURVE ( 'NONE', #12295, #9104, #868, .T. ) ;
#10909 = CARTESIAN_POINT ( 'NONE',  ( -9.085271536259636349, -21.17909668945641499, 56.44940867462261025 ) ) ;
#10910 = DIRECTION ( 'NONE',  ( -8.018662683283438208E-16, 5.975035461963189015E-16, 1.000000000000000000 ) ) ;
#10911 = DIRECTION ( 'NONE',  ( 0.000000000000000000, 0.000000000000000000, -1.000000000000000000 ) ) ;
#10912 = EDGE_CURVE ( 'NONE', #9643, #3619, #11697, .T. ) ;
#10913 = ORIENTED_EDGE ( 'NONE', *, *, #6341, .F. ) ;
#10914 = DIRECTION ( 'NONE',  ( 0.000000000000000000, 0.000000000000000000, -1.000000000000000000 ) ) ;
#10915 = CIRCLE ( 'NONE', #1631, 9.974999999999999645 ) ;
#10916 = CARTESIAN_POINT ( 'NONE',  ( -7.512805849530849400, -44.04964101872670312, -5.955427708867301106 ) ) ;
#10917 = ORIENTED_EDGE ( 'NONE', *, *, #787, .T. ) ;
#10918 = DIRECTION ( 'NONE',  ( -8.018662683283438208E-16, 5.975035461963189015E-16, 1.000000000000000000 ) ) ;
#10919 = ORIENTED_EDGE ( 'NONE', *, *, #2248, .F. ) ;
#10920 = CARTESIAN_POINT ( 'NONE',  ( -8.569834614884436874, -19.36726104528708703, 57.00231026484399166 ) ) ;
#10921 = VERTEX_POINT ( 'NONE', #12421 ) ;
#10922 = AXIS2_PLACEMENT_3D ( 'NONE', #13430, #3163, #6364 ) ;
#10923 = PRODUCT ( 'Tapered Toolholder Shank', 'Tapered Toolholder Shank', '', ( #7693 ) ) ;
#10924 = CARTESIAN_POINT ( 'NONE',  ( -9.760873592531986276, -5.348549538251085700, 56.85231026484398598 ) ) ;
#10925 = VECTOR ( 'NONE', #10843, 1000.000000000000000 ) ;
#10926 = ADVANCED_FACE ( 'NONE', ( #13715 ), #7805, .F. ) ;
#10927 = DIRECTION ( 'NONE',  ( 0.2536112499260171349, 0.9673062255102895524, -3.746065934159117949E-16 ) ) ;
#10928 = AXIS2_PLACEMENT_3D ( 'NONE', #6314, #1440, #2812 ) ;
#10929 = CARTESIAN_POINT ( 'NONE',  ( 13.85920135429429934, -27.00737899243800300, 43.21206422150100224 ) ) ;
#10930 = DIRECTION ( 'NONE',  ( 1.000000000000000000, 0.000000000000000000, 9.688619527525975741E-16 ) ) ;
#10931 = EDGE_CURVE ( 'NONE', #8222, #10056, #3592, .T. ) ;
#10932 = ORIENTED_EDGE ( 'NONE', *, *, #9202, .T. ) ;
#10933 = CARTESIAN_POINT ( 'NONE',  ( -11.49753086077415709, -51.43925603750204800, -17.78423269032954224 ) ) ;
#10934 = DIRECTION ( 'NONE',  ( 0.7071067811865473507, 0.7071067811865477948, 0.000000000000000000 ) ) ;
#10935 = VERTEX_POINT ( 'NONE', #10479 ) ;
#10936 = FACE_OUTER_BOUND ( 'NONE', #13281, .T. ) ;
#10937 = EDGE_LOOP ( 'NONE', ( #12218, #13326, #11628, #1233 ) ) ;
#10938 = CIRCLE ( 'NONE', #8244, 9.974999999999999645 ) ;
#10939 = CIRCLE ( 'NONE', #4595, 9.974999999999999645 ) ;
#10941 = ORIENTED_EDGE ( 'NONE', *, *, #5503, .F. ) ;
#10940 = DIRECTION ( 'NONE',  ( -8.018662683283438208E-16, 5.975035461963189015E-16, 1.000000000000000000 ) ) ;
#10942 = EDGE_CURVE ( 'NONE', #6707, #7319, #8, .T. ) ;
#10943 = ORIENTED_EDGE ( 'NONE', *, *, #558, .F. ) ;
#10944 = LINE ( 'NONE', #5200, #12270 ) ;
#10945 = AXIS2_PLACEMENT_3D ( 'NONE', #14129, #13975, #8301 ) ;
#10946 = LINE ( 'NONE', #5349, #3236 ) ;
#10947 = EDGE_LOOP ( 'NONE', ( #3919, #10119, #11945, #10959 ) ) ;
#10948 = DIRECTION ( 'NONE',  ( 0.000000000000000000, 0.1872998510044759646, 0.9823027872370621028 ) ) ;
#10949 = ADVANCED_FACE ( 'NONE', ( #7885 ), #83, .T. ) ;
#10950 = CARTESIAN_POINT ( 'NONE',  ( -10.48883820339395179, -4.847810977035234892, 61.37690497805530754 ) ) ;
#10951 = APPLICATION_PROTOCOL_DEFINITION ( 'draft international standard', 'automotive_design', 1998, #10759 ) ;
#10952 = EDGE_CURVE ( 'NONE', #8100, #9600, #6662, .T. ) ;
#10953 = AXIS2_PLACEMENT_3D ( 'NONE', #5414, #10076, #3123 ) ;
#10954 = AXIS2_PLACEMENT_3D ( 'NONE', #570, #14418, #6363 ) ;
#10955 = DIRECTION ( 'NONE',  ( -0.8018662683283436232, 0.5975035461963189576, -9.999999999999996833E-16 ) ) ;
#10956 = CIRCLE ( 'NONE', #12173, 8.314203600725839749 ) ;
#10957 = FACE_BOUND ( 'NONE', #14311, .T. ) ;
#10958 = CARTESIAN_POINT ( 'NONE',  ( -15.49969986081092088, -13.50737899243822504, 57.00231026484397745 ) ) ;
#10959 = ORIENTED_EDGE ( 'NONE', *, *, #7914, .F. ) ;
#10960 = FACE_BOUND ( 'NONE', #8315, .T. ) ;
#10962 = ORIENTED_EDGE ( 'NONE', *, *, #8945, .T. ) ;
#10961 = DIRECTION ( 'NONE',  ( 8.018662683283438208E-16, -5.975035461963189015E-16, -1.000000000000000000 ) ) ;
#10963 = VERTEX_POINT ( 'NONE', #8174 ) ;
#10964 = AXIS2_PLACEMENT_3D ( 'NONE', #12973, #14037, #2478 ) ;
#10965 = CARTESIAN_POINT ( 'NONE',  ( -15.49969986081092976, -95.55504406891904523, -9.828641771674195837 ) ) ;
#10966 = ORIENTED_EDGE ( 'NONE', *, *, #549, .T. ) ;
#10967 = CARTESIAN_POINT ( 'NONE',  ( -11.92312357957555236, -10.76045428471250709, -13.11735313252289181 ) ) ;
#10968 = CARTESIAN_POINT ( 'NONE',  ( -8.162984683111186968, -16.88054299694650595, 56.85231026484400019 ) ) ;
#10969 = CARTESIAN_POINT ( 'NONE',  ( -15.51120972694785749, -13.45872179377749589, 56.85231026484398598 ) ) ;
#10971 = CARTESIAN_POINT ( 'NONE',  ( -36.81454731355714216, 5.541088692458852272, 19.42860564753712538 ) ) ;
#10970 = DIRECTION ( 'NONE',  ( 0.5975035461963188466, 0.8018662683283437342, 0.000000000000000000 ) ) ;
#10972 = ORIENTED_EDGE ( 'NONE', *, *, #6847, .T. ) ;
#10973 = DIRECTION ( 'NONE',  ( -8.018662683283438208E-16, 5.975035461963189015E-16, 1.000000000000000000 ) ) ;
#10974 = VERTEX_POINT ( 'NONE', #3238 ) ;
#10975 = LINE ( 'NONE', #12351, #15065 ) ;
#10976 = ORIENTED_EDGE ( 'NONE', *, *, #3830, .T. ) ;
#10977 = ORIENTED_EDGE ( 'NONE', *, *, #2334, .F. ) ;
#10978 = CARTESIAN_POINT ( 'NONE',  ( -21.34246172570263411, -49.97817515884320017, 56.54480789128852791 ) ) ;
#10979 = ORIENTED_EDGE ( 'NONE', *, *, #12935, .T. ) ;
#10980 = VECTOR ( 'NONE', #14212, 1000.000000000000000 ) ;
#10982 = EDGE_CURVE ( 'NONE', #10775, #4535, #5523, .T. ) ;
#10981 = CYLINDRICAL_SURFACE ( 'NONE', #6396, 0.2000000000000012046 ) ;
#10983 = PLANE ( 'NONE',  #2561 ) ;
#10984 = CARTESIAN_POINT ( 'NONE',  ( -20.63946442839013784, -106.6916975368905156, -7.058995725539832122 ) ) ;
#10985 = CARTESIAN_POINT ( 'NONE',  ( -11.91594154455664700, -22.84528331856323291, 56.83039675413429848 ) ) ;
#10986 = AXIS2_PLACEMENT_3D ( 'NONE', #5337, #748, #14746 ) ;
#10987 = DIRECTION ( 'NONE',  ( -1.000000000000000000, -1.201369187114119994E-15, -9.616040805000176517E-16 ) ) ;
#10988 = DIRECTION ( 'NONE',  ( 0.000000000000000000, 0.000000000000000000, -1.000000000000000000 ) ) ;
#10989 = ORIENTED_EDGE ( 'NONE', *, *, #13109, .T. ) ;
#10990 = CARTESIAN_POINT ( 'NONE',  ( -35.49969986081099904, -19.50737899243800300, -7.509379629622798369 ) ) ;
#10991 = DIRECTION ( 'NONE',  ( 0.5975035461963188466, 0.8018662683283437342, 0.000000000000000000 ) ) ;
#10992 = ORIENTED_EDGE ( 'NONE', *, *, #9017, .F. ) ;
#10993 = CARTESIAN_POINT ( 'NONE',  ( 21.99139727573606606, -23.86149664705925488, 23.36879478108531316 ) ) ;
#10994 = LINE ( 'NONE', #2587, #4577 ) ;
#10995 = ORIENTED_EDGE ( 'NONE', *, *, #5943, .F. ) ;
#10996 = DIRECTION ( 'NONE',  ( -0.9673062255102896634, 0.2536112499260171904, -9.271838545667876730E-16 ) ) ;
#10997 = ORIENTED_EDGE ( 'NONE', *, *, #934, .T. ) ;
#10998 = EDGE_CURVE ( 'NONE', #6817, #14904, #14861, .T. ) ;
#10999 = CARTESIAN_POINT ( 'NONE',  ( -15.49969986081099549, -2.007378992438005216, 52.21206422150100224 ) ) ;
#11000 = CARTESIAN_POINT ( 'NONE',  ( -15.49969986081092088, -13.50737899243822504, 57.00231026484397745 ) ) ;
#11001 = AXIS2_PLACEMENT_3D ( 'NONE', #5611, #2026, #6968 ) ;
#11002 = LINE ( 'NONE', #13088, #11876 ) ;
#11003 = DIRECTION ( 'NONE',  ( -1.000000000000000000, 0.000000000000000000, 0.000000000000000000 ) ) ;
#11004 = VERTEX_POINT ( 'NONE', #6509 ) ;
#11005 = CARTESIAN_POINT ( 'NONE',  ( -32.87720281798463873, 9.589597845032626466, 31.89482592002004679 ) ) ;
#11006 = DIRECTION ( 'NONE',  ( 0.9931883319083343320, -0.1165201156931293391, 8.660254037844386422E-16 ) ) ;
#11007 = VERTEX_POINT ( 'NONE', #14713 ) ;
#11008 = ORIENTED_EDGE ( 'NONE', *, *, #9145, .T. ) ;
#11010 = ORIENTED_EDGE ( 'NONE', *, *, #3284, .T. ) ;
#11009 = CYLINDRICAL_SURFACE ( 'NONE', #2533, 5.371426149148541107 ) ;
#11011 = ORIENTED_EDGE ( 'NONE', *, *, #5297, .F. ) ;
#11012 = ADVANCED_FACE ( 'NONE', ( #4235 ), #7733, .T. ) ;
#11013 = FACE_OUTER_BOUND ( 'NONE', #8547, .T. ) ;
#11014 = VERTEX_POINT ( 'NONE', #1221 ) ;
#11015 = EDGE_CURVE ( 'NONE', #1385, #8470, #7010, .T. ) ;
#11016 = CARTESIAN_POINT ( 'NONE',  ( -24.28571865450477674, -8.784403367172062715, 57.00231026484397745 ) ) ;
#11017 = CARTESIAN_POINT ( 'NONE',  ( -7.838622488183276893, -46.81654903479443419, -3.012281934724219123 ) ) ;
#11018 = CARTESIAN_POINT ( 'NONE',  ( -15.49969986081099904, -26.50737899243800655, 57.00231026484399877 ) ) ;
#11019 = AXIS2_PLACEMENT_3D ( 'NONE', #12524, #10296, #4419 ) ;
#11020 = DIRECTION ( 'NONE',  ( 0.5975035461963188466, 0.8018662683283437342, 0.000000000000000000 ) ) ;
#11021 = LINE ( 'NONE', #6420, #9592 ) ;
#11022 = VERTEX_POINT ( 'NONE', #355 ) ;
#11023 = CARTESIAN_POINT ( 'NONE',  ( -15.14850084941412511, -4.438867027711355107, 56.85231026484398598 ) ) ;
#11024 = ORIENTED_EDGE ( 'NONE', *, *, #7088, .F. ) ;
#11025 = LINE ( 'NONE', #2774, #6073 ) ;
#11026 = ORIENTED_EDGE ( 'NONE', *, *, #14674, .T. ) ;
#11027 = VERTEX_POINT ( 'NONE', #2710 ) ;
#11028 = EDGE_CURVE ( 'NONE', #2807, #7478, #10665, .T. ) ;
#11029 = PLANE ( 'NONE',  #6520 ) ;
#11030 = ADVANCED_FACE ( 'NONE', ( #7135 ), #7364, .F. ) ;
#11031 = ORIENTED_EDGE ( 'NONE', *, *, #9440, .T. ) ;
#11032 = VECTOR ( 'NONE', #2077, 1000.000000000000000 ) ;
#11033 = DIRECTION ( 'NONE',  ( -8.018662683283438208E-16, 5.975035461963189015E-16, 1.000000000000000000 ) ) ;
#11034 = LINE ( 'NONE', #8734, #10513 ) ;
#11035 = CARTESIAN_POINT ( 'NONE',  ( -7.506093261461533217, -14.65346081099998088, 56.85231026484400019 ) ) ;
#11036 = B_SPLINE_CURVE_WITH_KNOTS ( 'NONE', 3,
 ( #3222, #11558, #10255, #5738, #3524, #5658, #4602, #12564, #9026, #11332, #9103, #9330, #3303, #10330, #9255, #14851, #6945, #13855, #13931, #3446, #8098, #12797, #2307, #6649, #5812, #11627, #14006, #10171 ),
 .UNSPECIFIED., .F., .F.,
 ( 4, 2, 2, 2, 2, 2, 1, 2, 2, 2, 2, 1, 2, 2, 4 ),
 ( 0.1453386670947538206, 0.1675069210422008015, 0.1785910480159242086, 0.1896751749896476158, 0.2340116828845410779, 0.2561799368319878090, 0.2783481907794345123, 0.3005164447268813266, 0.3226846986743281409, 0.3670212065692216030, 0.3891894605166682508, 0.4113577144641149541, 0.4335259684115615464, 0.4556942223590082497, 0.5000307302539015453 ),
 .UNSPECIFIED. ) ;
#11037 =( REPRESENTATION_RELATIONSHIP ('NONE','NONE', #2372, #2852 ) REPRESENTATION_RELATIONSHIP_WITH_TRANSFORMATION ( #10379 )SHAPE_REPRESENTATION_RELATIONSHIP( ) );
#11038 = VECTOR ( 'NONE', #8202, 1000.000000000000000 ) ;
#11039 = VECTOR ( 'NONE', #5661, 1000.000000000000000 ) ;
#11040 = PRODUCT_DEFINITION_SHAPE ( 'NONE', 'NONE',  #11525 ) ;
#11041 = CIRCLE ( 'NONE', #1526, 2.000000000000001776 ) ;
#11043 = DIRECTION ( 'NONE',  ( -0.8719950447285823580, -0.4895147004624046394, -4.067366430758000189E-16 ) ) ;
#11042 = CARTESIAN_POINT ( 'NONE',  ( -12.51218212982931810, -9.498047650796513253, 45.50231026484398456 ) ) ;
#11044 = ORIENTED_EDGE ( 'NONE', *, *, #12874, .T. ) ;
#11045 = DIRECTION ( 'NONE',  ( -8.018662683283438208E-16, 5.975035461963189015E-16, 1.000000000000000000 ) ) ;
#11046 = VERTEX_POINT ( 'NONE', #9595 ) ;
#11047 = LINE ( 'NONE', #14567, #4821 ) ;
#11048 = ORIENTED_EDGE ( 'NONE', *, *, #4995, .F. ) ;
#11049 = EDGE_LOOP ( 'NONE', ( #5238, #1696, #13357, #3823 ) ) ;
#11050 = CARTESIAN_POINT ( 'NONE',  ( -33.49969986081099904, -51.00737899243799944, 52.39987856403599409 ) ) ;
#11051 = EDGE_CURVE ( 'NONE', #3278, #1260, #9028, .T. ) ;
#11052 = ORIENTED_EDGE ( 'NONE', *, *, #14764, .F. ) ;
#11053 = DIRECTION ( 'NONE',  ( 0.2196982563774082797, 0.9755678736739573642, -4.067366430757958773E-16 ) ) ;
#11054 = CIRCLE ( 'NONE', #4457, 9.974999999999999645 ) ;
#11055 = EDGE_CURVE ( 'NONE', #1609, #7946, #5644, .T. ) ;
#11056 = VECTOR ( 'NONE', #2592, 1000.000000000000000 ) ;
#11057 = CIRCLE ( 'NONE', #14968, 9.974999999999999645 ) ;
#11058 = VECTOR ( 'NONE', #6955, 1000.000000000000000 ) ;
#11059 = CARTESIAN_POINT ( 'NONE',  ( 7.200737182676100190, 4.873818854045000037, 20.51204286552489009 ) ) ;
#11060 = PLANE ( 'NONE',  #7563 ) ;
#11061 = CARTESIAN_POINT ( 'NONE',  ( -31.79969986081099975, 20.99262100756200056, 16.16206422150100153 ) ) ;
#11062 = PRODUCT_RELATED_PRODUCT_CATEGORY ( 'part', '', ( #4461 ) ) ;
#11063 = EDGE_CURVE ( 'NONE', #4396, #10787, #196, .T. ) ;
#11064 = CARTESIAN_POINT ( 'NONE',  ( -23.49969986081099904, -44.50737899243799944, 19.50231026484399877 ) ) ;
#11065 = CYLINDRICAL_SURFACE ( 'NONE', #13292, 3.000000000000002665 ) ;
#11066 = VERTEX_POINT ( 'NONE', #11974 ) ;
#11067 = DIRECTION ( 'NONE',  ( -1.000000000000000000, -3.839882694219489529E-17, 0.000000000000000000 ) ) ;
#11068 = LINE ( 'NONE', #591, #4862 ) ;
#11069 = ORIENTED_EDGE ( 'NONE', *, *, #7186, .F. ) ;
#11070 = VECTOR ( 'NONE', #5961, 1000.000000000000000 ) ;
#11071 = DIRECTION ( 'NONE',  ( 0.08178736187250883194, 0.9966498018049948504, -5.299192642332142575E-16 ) ) ;
#11072 = VERTEX_POINT ( 'NONE', #9672 ) ;
#11073 = CARTESIAN_POINT ( 'NONE',  ( -21.11416342254291934, -20.63752968607602867, 57.00231026484397745 ) ) ;
#11074 = EDGE_LOOP ( 'NONE', ( #738, #9554, #3545, #14081 ) ) ;
#11075 = CARTESIAN_POINT ( 'NONE',  ( 2.500300139188999182, -42.00737899243800655, -13.39525803434800011 ) ) ;
#11076 = CARTESIAN_POINT ( 'NONE',  ( -18.48721759179251123, -17.51671033407994926, 51.00031026484398922 ) ) ;
#11077 = VECTOR ( 'NONE', #2814, 1000.000000000000000 ) ;
#11078 = CARTESIAN_POINT ( 'NONE',  ( -7.499751500627867884, -49.00722532478560822, 19.47034365934475275 ) ) ;
#11079 = EDGE_CURVE ( 'NONE', #2590, #5603, #3856, .T. ) ;
#11080 = CARTESIAN_POINT ( 'NONE',  ( -15.49969986081099904, 64.39262100756199914, 30.46206422150100934 ) ) ;
#11081 = CARTESIAN_POINT ( 'NONE',  ( -15.53608329785963527, -13.54167542823733328, 56.85231026484398598 ) ) ;
#11082 = ORIENTED_EDGE ( 'NONE', *, *, #4560, .T. ) ;
#11083 = CARTESIAN_POINT ( 'NONE',  ( -15.49969986081099194, -110.2236589786222538, -11.14993866902398700 ) ) ;
#11084 = LINE ( 'NONE', #4123, #923 ) ;
#11085 = ORIENTED_EDGE ( 'NONE', *, *, #12207, .T. ) ;
#11086 = ORIENTED_EDGE ( 'NONE', *, *, #3733, .T. ) ;
#11088 = EDGE_LOOP ( 'NONE', ( #2952, #8686, #11802, #5657 ) ) ;
#11087 = CARTESIAN_POINT ( 'NONE',  ( -34.57446802530316887, -38.90440891063803974, -12.78416974581375065 ) ) ;
#11089 = ORIENTED_EDGE ( 'NONE', *, *, #729, .F. ) ;
#11090 = AXIS2_PLACEMENT_3D ( 'NONE', #7689, #1817, #13523 ) ;
#11091 = DIRECTION ( 'NONE',  ( -8.018662683283438208E-16, 5.975035461963189015E-16, 1.000000000000000000 ) ) ;
#11092 = CARTESIAN_POINT ( 'NONE',  ( 7.000300139189000070, -32.00737899243799944, -5.787935778498998651 ) ) ;
#11093 = DIRECTION ( 'NONE',  ( 0.9805849309054470719, 0.1960948578651654506, 6.691306063588581484E-16 ) ) ;
#11094 = CARTESIAN_POINT ( 'NONE',  ( -33.37394235882850069, 7.183219930803497633, 17.76912582958182085 ) ) ;
#11095 = AXIS2_PLACEMENT_3D ( 'NONE', #14731, #1180, #9285 ) ;
#11096 = CARTESIAN_POINT ( 'NONE',  ( -24.21370508435883551, -8.652820519829271362, 54.00231026484397745 ) ) ;
#11097 = FACE_OUTER_BOUND ( 'NONE', #13043, .T. ) ;
#11098 = CIRCLE ( 'NONE', #6677, 9.974999999999999645 ) ;
#11099 = EDGE_CURVE ( 'NONE', #4500, #3108, #9055, .T. ) ;
#11100 = LINE ( 'NONE', #12477, #6998 ) ;
#11101 = DIRECTION ( 'NONE',  ( 0.000000000000000000, 1.224646799147350002E-16, -1.000000000000000000 ) ) ;
#11102 = EDGE_CURVE ( 'NONE', #11853, #9110, #4685, .T. ) ;
#11103 = ORIENTED_EDGE ( 'NONE', *, *, #13153, .T. ) ;
#11104 = DIRECTION ( 'NONE',  ( -0.8415927028326163351, 0.5401126942952662047, -9.975640502598247923E-16 ) ) ;
#11105 = VERTEX_POINT ( 'NONE', #14488 ) ;
#11106 = CARTESIAN_POINT ( 'NONE',  ( -15.49969986081099194, -110.0808295834072652, -11.13818985276707707 ) ) ;
#11108 = ORIENTED_EDGE ( 'NONE', *, *, #14021, .F. ) ;
#11107 = CARTESIAN_POINT ( 'NONE',  ( -14.15531688186919723, -11.70317988869945580, 51.00231026484399166 ) ) ;
#11109 = ORIENTED_EDGE ( 'NONE', *, *, #656, .F. ) ;
#11110 = DIRECTION ( 'NONE',  ( 0.000000000000000000, -1.000000000000000000, -1.224646799147350002E-16 ) ) ;
#11112 = EDGE_LOOP ( 'NONE', ( #5217, #1443, #6012, #9261 ) ) ;
#11111 = DIRECTION ( 'NONE',  ( -8.018662683283438208E-16, 5.975035461963189015E-16, 1.000000000000000000 ) ) ;
#11113 = CARTESIAN_POINT ( 'NONE',  ( -14.04785070661220736, -9.237812854699480880, -13.26081354841219451 ) ) ;
#11114 = VECTOR ( 'NONE', #3832, 1000.000000000000000 ) ;
#11115 = DIRECTION ( 'NONE',  ( -1.224646799147350002E-16, -1.224646799147350002E-16, 1.000000000000000000 ) ) ;
#11116 = LINE ( 'NONE', #13274, #11946 ) ;
#11117 = EDGE_CURVE ( 'NONE', #1266, #13484, #14716, .T. ) ;
#11118 = EDGE_CURVE ( 'NONE', #11355, #14421, #1991, .T. ) ;
#11119 = AXIS2_PLACEMENT_3D ( 'NONE', #10643, #3687, #3531 ) ;
#11121 = CARTESIAN_POINT ( 'NONE',  ( -35.91640051037089165, 5.971976172174843001, 18.89405436573536079 ) ) ;
#11120 = DIRECTION ( 'NONE',  ( -0.2196982563774038943, -0.9755678736739584744, 4.067366430757998709E-16 ) ) ;
#11122 = ADVANCED_FACE ( 'NONE', ( #8962 ), #5378, .T. ) ;
#11123 = ORIENTED_EDGE ( 'NONE', *, *, #14663, .T. ) ;
#11124 = LINE ( 'NONE', #719, #14604 ) ;
#11125 = VERTEX_POINT ( 'NONE', #6581 ) ;
#11126 = LINE ( 'NONE', #14493, #908 ) ;
#11127 = ORIENTED_EDGE ( 'NONE', *, *, #1865, .T. ) ;
#11128 = ORIENTED_EDGE ( 'NONE', *, *, #6429, .T. ) ;
#11129 = CARTESIAN_POINT ( 'NONE',  ( 21.85920135429434907, -27.00737899243800300, 20.96206422150100224 ) ) ;
#11130 = CARTESIAN_POINT ( 'NONE',  ( -15.49969986081092088, -13.50737899243822504, 56.85231026484398598 ) ) ;
#11131 = ORIENTED_EDGE ( 'NONE', *, *, #6341, .T. ) ;
#11132 = ADVANCED_FACE ( 'NONE', ( #497 ), #4009, .F. ) ;
#11133 = CARTESIAN_POINT ( 'NONE',  ( -14.45138012959125184, -36.57197769750143124, 56.98857378514258443 ) ) ;
#11134 = CARTESIAN_POINT ( 'NONE',  ( -15.11203582817000068, -107.1622034095870077, -6.087689735156000204 ) ) ;
#11135 = CARTESIAN_POINT ( 'NONE',  ( -14.61203582817000068, -107.5837463816240529, -4.877506371889843706 ) ) ;
#11136 = EDGE_CURVE ( 'NONE', #3490, #13967, #14443, .T. ) ;
#11137 = CARTESIAN_POINT ( 'NONE',  ( -15.49969986081099904, -36.50737899243799944, 57.00231026484399877 ) ) ;
#11138 = EDGE_CURVE ( 'NONE', #9794, #337, #9962, .T. ) ;
#11139 = B_SPLINE_CURVE_WITH_KNOTS ( 'NONE', 3,
 ( #11260, #780, #5439, #8952 ),
 .UNSPECIFIED., .F., .F.,
 ( 4, 4 ),
 ( 0.8772132959648567541, 1.000000000000000000 ),
 .UNSPECIFIED. ) ;
#11140 = FACE_BOUND ( 'NONE', #7481, .T. ) ;
#11141 = CARTESIAN_POINT ( 'NONE',  ( -5.499699860811003482, -46.50737899243799944, 44.50231026484399877 ) ) ;
#11142 = ORIENTED_EDGE ( 'NONE', *, *, #13236, .F. ) ;
#11143 = CARTESIAN_POINT ( 'NONE',  ( -18.09969986081091875, -107.1622034095862972, -6.087689735156002868 ) ) ;
#11144 = DIRECTION ( 'NONE',  ( 0.5975035461963188466, 0.8018662683283437342, 0.000000000000000000 ) ) ;
#11145 = EDGE_LOOP ( 'NONE', ( #1478, #9063, #10783, #14353 ) ) ;
#11146 = CARTESIAN_POINT ( 'NONE',  ( -5.499699860811003482, -46.50737899243799944, 44.50231026484399877 ) ) ;
#11147 = VECTOR ( 'NONE', #11154, 1000.000000000000000 ) ;
#11148 = DIRECTION ( 'NONE',  ( 0.1617534816134024167, -0.9868311969055004740, 7.193398003386505973E-16 ) ) ;
#11149 = ORIENTED_EDGE ( 'NONE', *, *, #12346, .F. ) ;
#11150 = DIRECTION ( 'NONE',  ( 0.000000000000000000, 1.000000000000000000, 1.224646799147350002E-16 ) ) ;
#11151 = EDGE_CURVE ( 'NONE', #10963, #10056, #9821, .T. ) ;
#11152 = LINE ( 'NONE', #9920, #7306 ) ;
#11153 = CARTESIAN_POINT ( 'NONE',  ( -17.61203582817000068, -106.9280785958314368, -4.859811251109668717 ) ) ;
#11154 = DIRECTION ( 'NONE',  ( -8.018662683283438208E-16, 5.975035461963189015E-16, 1.000000000000000000 ) ) ;
#11155 = CARTESIAN_POINT ( 'NONE',  ( -7.223083447440863836, -17.23012942000294245, 57.00231026484399166 ) ) ;
#11156 = VERTEX_POINT ( 'NONE', #795 ) ;
#11157 = CARTESIAN_POINT ( 'NONE',  ( -33.10531216574866420, 8.250019247744555528, 31.36164418743403459 ) ) ;
#11158 = CARTESIAN_POINT ( 'NONE',  ( -7.586235653186040651, -45.66775839773830370, -3.133043233650827375 ) ) ;
#11159 = CIRCLE ( 'NONE', #654, 37.50000000000000711 ) ;
#11160 = ORIENTED_EDGE ( 'NONE', *, *, #13100, .F. ) ;
#11162 = ORIENTED_EDGE ( 'NONE', *, *, #2264, .T. ) ;
#11161 = DIRECTION ( 'NONE',  ( -8.018662683283438208E-16, 5.975035461963189015E-16, 1.000000000000000000 ) ) ;
#11163 = VERTEX_POINT ( 'NONE', #11042 ) ;
#11164 = CARTESIAN_POINT ( 'NONE',  ( -7.886584594865169606, -46.96511696614940234, 21.96004823855531640 ) ) ;
#11165 = VECTOR ( 'NONE', #7240, 1000.000000000000000 ) ;
#11166 = LINE ( 'NONE', #11389, #10710 ) ;
#11167 = EDGE_CURVE ( 'NONE', #14533, #4396, #3701, .T. ) ;
#11168 = EDGE_CURVE ( 'NONE', #8839, #9541, #13573, .T. ) ;
#11169 = CARTESIAN_POINT ( 'NONE',  ( -16.41401162527548507, -4.478243707298169340, 56.85231026484398598 ) ) ;
#11170 = CARTESIAN_POINT ( 'NONE',  ( -8.710519834377311810, -48.73976024287854614, 45.63987292668604567 ) ) ;
#11171 = PRODUCT ( 'Cross Slide Block', 'Cross Slide Block', '', ( #7770 ) ) ;
#11172 = DIRECTION ( 'NONE',  ( -1.000000000000000000, 0.000000000000000000, 0.000000000000000000 ) ) ;
#11173 = CARTESIAN_POINT ( 'NONE',  ( -9.989347722329673829, -46.50737899243799944, -5.497689735156000346 ) ) ;
#11174 = DIRECTION ( 'NONE',  ( -0.6519834208811554621, -0.7582332219680868457, -6.975647374412761332E-17 ) ) ;
#11175 = AXIS2_PLACEMENT_3D ( 'NONE', #13463, #756, #606 ) ;
#11176 = CARTESIAN_POINT ( 'NONE',  ( -38.46438895118065915, 4.086072560925112285, 22.89991886225540796 ) ) ;
#11177 = CARTESIAN_POINT ( 'NONE',  ( -7.515340099725619005, -44.00737978687738661, 44.36832752824940940 ) ) ;
#11178 = AXIS2_PLACEMENT_3D ( 'NONE', #6948, #10608, #11831 ) ;
#11179 = ORIENTED_EDGE ( 'NONE', *, *, #9855, .T. ) ;
#11180 = CARTESIAN_POINT ( 'NONE',  ( 14.70450431974454020, -27.46836090773456007, 46.43726578852947995 ) ) ;
#11181 = VERTEX_POINT ( 'NONE', #7593 ) ;
#11182 = DIRECTION ( 'NONE',  ( -0.8934395198752397294, 0.4491835085186243748, -9.848077530122081084E-16 ) ) ;
#11184 = VERTEX_POINT ( 'NONE', #6438 ) ;
#11183 = CARTESIAN_POINT ( 'NONE',  ( -7.512159534862917099, -44.97983827236478049, -7.479109963946024564 ) ) ;
#11185 = EDGE_LOOP ( 'NONE', ( #5776, #13907, #13706, #2081 ) ) ;
#11186 = LINE ( 'NONE', #7876, #15085 ) ;
#11188 = ORIENTED_EDGE ( 'NONE', *, *, #4963, .T. ) ;
#11187 = LINE ( 'NONE', #3871, #8153 ) ;
#11189 = CARTESIAN_POINT ( 'NONE',  ( -7.691420491076302213, -11.44776172600821340, 56.85231026484400019 ) ) ;
#11190 = ADVANCED_FACE ( 'NONE', ( #12194 ), #1709, .T. ) ;
#11191 = VECTOR ( 'NONE', #12849, 999.9999999999998863 ) ;
#11192 = VECTOR ( 'NONE', #7909, 1000.000000000000000 ) ;
#11193 = CARTESIAN_POINT ( 'NONE',  ( -18.09969986081100046, -107.2302401527028337, -7.385908130336948929 ) ) ;
#11194 = CIRCLE ( 'NONE', #4598, 9.974999999999999645 ) ;
#11195 = LINE ( 'NONE', #564, #705 ) ;
#11196 = DIRECTION ( 'NONE',  ( -1.000000000000000000, 1.291538348938060198E-32, -1.054621095516909827E-16 ) ) ;
#11197 = DIRECTION ( 'NONE',  ( 1.000000000000000000, 1.201369187114119994E-15, 9.616040805000176517E-16 ) ) ;
#11198 = VERTEX_POINT ( 'NONE', #8894 ) ;
#11199 = DIRECTION ( 'NONE',  ( 0.6780482080269577549, 0.7350174335289139105, 1.045284632676540317E-16 ) ) ;
#11200 = DIRECTION ( 'NONE',  ( 0.000000000000000000, -1.000000000000000000, -1.224646799147350002E-16 ) ) ;
#11201 = ORIENTED_EDGE ( 'NONE', *, *, #1583, .F. ) ;
#11202 = VERTEX_POINT ( 'NONE', #5231 ) ;
#11203 = CIRCLE ( 'NONE', #953, 6.250000000000001776 ) ;
#11204 = CARTESIAN_POINT ( 'NONE',  ( -3.508527451664998686, -47.37340439622244048, -6.997689735156000346 ) ) ;
#11205 = ORIENTED_EDGE ( 'NONE', *, *, #11311, .F. ) ;
#11206 = B_SPLINE_CURVE_WITH_KNOTS ( 'NONE', 3,
 ( #2135, #6930, #12544, #8080, #11614, #1130, #10238, #911, #9085, #5792 ),
 .UNSPECIFIED., .F., .F.,
 ( 4, 2, 2, 2, 4 ),
 ( 0.000000000000000000, 0.0005821621410504860704, 0.001164324282100972141, 0.001746486423151458103, 0.002328648564201944281 ),
 .UNSPECIFIED. ) ;
#11207 = FACE_OUTER_BOUND ( 'NONE', #3954, .T. ) ;
#11208 = ADVANCED_FACE ( 'NONE', ( #12272 ), #5450, .F. ) ;
#11209 = B_SPLINE_CURVE_WITH_KNOTS ( 'NONE', 3,
 ( #1103, #5761, #10432, #15100, #6969, #4401, #9128, #9051, #7818, #12506, #5612, #3255, #12590, #11432, #959, #13807, #3324, #40, #10819, #4859, #3704, #1179, #7052, #10512, #1336, #269, #2410, #3552, #3854, #5908, #9437, #1486, #2559, #11729, #2705, #7129, #13203, #1252, #7208 ),
 .UNSPECIFIED., .F., .F.,
 ( 4, 2, 1, 1, 1, 2, 2, 2, 2, 1, 1, 1, 1, 2, 2, 2, 2, 1, 1, 1, 1, 2, 2, 2, 4 ),
 ( 0.5684180336906330400, 0.5701039007465288355, 0.5717897678024245200, 0.5751615019142162222, 0.5819049701377994044, 0.5953919065849659908, 0.6223657794792989417, 0.6763135252679648435, 0.6771564587959129078, 0.6779993923238609721, 0.6796852593797569897, 0.6830569934915491359, 0.6898004617151334283, 0.7032873981623020132, 0.7302612710566397380, 0.7842090168453148546, 0.7850519503732626969, 0.7858948839012106502, 0.7875807509571066678, 0.7909524850688987030, 0.7976959532924827734, 0.8111828897396505811, 0.8381567626339864185, 0.8921045084226580935, 1.000000000000000000 ),
 .UNSPECIFIED. ) ;
#11210 = VECTOR ( 'NONE', #420, 1000.000000000000000 ) ;
#11211 = ADVANCED_FACE ( 'NONE', ( #9894 ), #8738, .F. ) ;
#11212 = DIRECTION ( 'NONE',  ( 0.9354976265738677021, -0.3533329742249661232, 9.612616959383195326E-16 ) ) ;
#11213 = CARTESIAN_POINT ( 'NONE',  ( -23.39388780995641781, -11.80648316271623877, 56.85231026484398598 ) ) ;
#11214 = AXIS2_PLACEMENT_3D ( 'NONE', #3983, #14538, #14392 ) ;
#11215 = FACE_OUTER_BOUND ( 'NONE', #2638, .T. ) ;
#11216 = DIRECTION ( 'NONE',  ( -1.000000000000000078E-15, 1.000000000000000000, 0.000000000000000000 ) ) ;
#11217 = ORIENTED_EDGE ( 'NONE', *, *, #14390, .T. ) ;
#11218 = CARTESIAN_POINT ( 'NONE',  ( -15.61203582816999891, -107.5495670694337207, -7.066625679870576882 ) ) ;
#11219 = CIRCLE ( 'NONE', #11454, 0.4500000000000011768 ) ;
#11220 = FACE_OUTER_BOUND ( 'NONE', #3218, .T. ) ;
#11221 = VERTEX_POINT ( 'NONE', #14788 ) ;
#11222 = FACE_OUTER_BOUND ( 'NONE', #5154, .T. ) ;
#11223 = DIRECTION ( 'NONE',  ( 1.000000000000000000, 1.000000000000000078E-15, 0.000000000000000000 ) ) ;
#11224 = LINE ( 'NONE', #9068, #3274 ) ;
#11225 = VERTEX_POINT ( 'NONE', #716 ) ;
#11226 = CARTESIAN_POINT ( 'NONE',  ( 9.000300139189000959, -32.00737899243799944, -4.178074911655800250 ) ) ;
#11227 = ADVANCED_FACE ( 'NONE', ( #13498 ), #3008, .F. ) ;
#11228 = EDGE_CURVE ( 'NONE', #13230, #1495, #4309, .T. ) ;
#11229 = CARTESIAN_POINT ( 'NONE',  ( -15.49969986081099904, 64.39262100756199914, 17.96206422150100579 ) ) ;
#11230 = VECTOR ( 'NONE', #3151, 1000.000000000000000 ) ;
#11231 = CIRCLE ( 'NONE', #12953, 3.249999999999999556 ) ;
#11232 = APPLICATION_PROTOCOL_DEFINITION ( 'draft international standard', 'automotive_design', 1998, #9961 ) ;
#11233 = CARTESIAN_POINT ( 'NONE',  ( -7.749729581312787552, -48.02091033735556636, 21.51272064359849168 ) ) ;
#11234 = CARTESIAN_POINT ( 'NONE',  ( -15.49969986081099904, -52.50737899243800655, -13.49768973515600656 ) ) ;
#11235 = DIRECTION ( 'NONE',  ( -0.9547156899063192759, -0.2975196656469966672, -5.877852522924767272E-16 ) ) ;
#11236 = VERTEX_POINT ( 'NONE', #3458 ) ;
#11237 = CARTESIAN_POINT ( 'NONE',  ( -33.37394235882850069, 7.183219930803497633, 30.65500261342018007 ) ) ;
#11238 = DIRECTION ( 'NONE',  ( -0.7109061395677416240, 0.7032868978765995926, -9.902680687415702019E-16 ) ) ;
#11239 = ORIENTED_EDGE ( 'NONE', *, *, #747, .T. ) ;
#11241 = ORIENTED_EDGE ( 'NONE', *, *, #7434, .F. ) ;
#11240 = LINE ( 'NONE', #1907, #1802 ) ;
#11242 = ORIENTED_EDGE ( 'NONE', *, *, #8553, .F. ) ;
#11243 = DIRECTION ( 'NONE',  ( 8.018662683283438208E-16, -5.975035461963189015E-16, -1.000000000000000000 ) ) ;
#11244 = CARTESIAN_POINT ( 'NONE',  ( -10.83521803515972159, -51.01205933293365291, 56.71172365652226688 ) ) ;
#11245 = EDGE_CURVE ( 'NONE', #4906, #13839, #12808, .T. ) ;
#11246 = AXIS2_PLACEMENT_3D ( 'NONE', #7437, #3929, #10892 ) ;
#11247 = DIRECTION ( 'NONE',  ( -0.5975035461963187355, -0.8018662683283438453, 0.000000000000000000 ) ) ;
#11248 = CARTESIAN_POINT ( 'NONE',  ( -8.309331736433431814, -48.01736933888442849, 46.50111227020314431 ) ) ;
#11249 = LINE ( 'NONE', #921, #5773 ) ;
#11250 = CARTESIAN_POINT ( 'NONE',  ( 9.000300139189000959, -32.00737899243799944, 52.60220335465780295 ) ) ;
#11251 = CARTESIAN_POINT ( 'NONE',  ( -8.162984683111186968, -16.88054299694650595, 56.85231026484400019 ) ) ;
#11252 = ADVANCED_FACE ( 'NONE', ( #13716 ), #946, .F. ) ;
#11253 = CARTESIAN_POINT ( 'NONE',  ( -7.594860258898399330, -10.18326093375929631, 56.85231026484400019 ) ) ;
#11254 = CARTESIAN_POINT ( 'NONE',  ( 15.51282817721622109, -29.51029345576456819, 45.29537398124922021 ) ) ;
#11255 = VECTOR ( 'NONE', #329, 1000.000000000000000 ) ;
#11256 = VERTEX_POINT ( 'NONE', #3390 ) ;
#11258 = ORIENTED_EDGE ( 'NONE', *, *, #7681, .T. ) ;
#11257 = DIRECTION ( 'NONE',  ( -8.018662683283438208E-16, 5.975035461963189015E-16, 1.000000000000000000 ) ) ;
#11259 = ORIENTED_EDGE ( 'NONE', *, *, #619, .F. ) ;
#11260 = CARTESIAN_POINT ( 'NONE',  ( -7.754796638793765240, -46.50763592918296752, 17.00313569000094560 ) ) ;
#11262 = ORIENTED_EDGE ( 'NONE', *, *, #10743, .F. ) ;
#11261 = CARTESIAN_POINT ( 'NONE',  ( 1.877803096367266278, 9.589597844970082718, 16.52930252299240621 ) ) ;
#11263 = CARTESIAN_POINT ( 'NONE',  ( -20.87112600995945755, -109.7258744763782943, -5.497689735156006563 ) ) ;
#11264 = DIRECTION ( 'NONE',  ( -8.018662683283438208E-16, 5.975035461963189015E-16, 1.000000000000000000 ) ) ;
#11265 = CARTESIAN_POINT ( 'NONE',  ( -7.795459123704181259, -47.76474896896235123, -7.658500196163376295 ) ) ;
#11266 = EDGE_CURVE ( 'NONE', #1475, #14941, #557, .T. ) ;
#11267 = DIRECTION ( 'NONE',  ( 8.018662683283438208E-16, -5.975035461963189015E-16, -1.000000000000000000 ) ) ;
#11268 = ORIENTED_EDGE ( 'NONE', *, *, #997, .T. ) ;
#11269 = CARTESIAN_POINT ( 'NONE',  ( 18.47578936866889876, -26.09629254026139122, 40.08401990837758433 ) ) ;
#11270 = ORIENTED_EDGE ( 'NONE', *, *, #8676, .F. ) ;
#11271 = DIRECTION ( 'NONE',  ( 0.7071067811865475727, -0.7071067811865475727, -1.202263280131018653E-17 ) ) ;
#11272 = VERTEX_POINT ( 'NONE', #12729 ) ;
#11273 = ORIENTED_EDGE ( 'NONE', *, *, #11411, .F. ) ;
#11274 = VECTOR ( 'NONE', #13206, 1000.000000000000227 ) ;
#11275 = FACE_OUTER_BOUND ( 'NONE', #10420, .T. ) ;
#11276 = ORIENTED_EDGE ( 'NONE', *, *, #3647, .T. ) ;
#11277 = CARTESIAN_POINT ( 'NONE',  ( -10.21615383005687505, -38.47745445305465495, 56.63013494352767907 ) ) ;
#11278 = CARTESIAN_POINT ( 'NONE',  ( -23.05384319539488658, -10.65421522557165623, 56.85231026484398598 ) ) ;
#11279 = CIRCLE ( 'NONE', #4450, 19.00000000000000000 ) ;
#11280 = DIRECTION ( 'NONE',  ( 0.000000000000000000, 0.1872998510044689147, 0.9823027872370635460 ) ) ;
#11281 = VECTOR ( 'NONE', #3522, 1000.000000000000000 ) ;
#11282 = CARTESIAN_POINT ( 'NONE',  ( 4.806612929223899044, 12.32432269367079591, 16.16206422150100153 ) ) ;
#11283 = CARTESIAN_POINT ( 'NONE',  ( -38.49969986081099904, -37.00737899243799944, 49.12071670408379731 ) ) ;
#11284 = EDGE_CURVE ( 'NONE', #8725, #7674, #12655, .T. ) ;
#11286 = CYLINDRICAL_SURFACE ( 'NONE', #1184, 0.3999999999999998557 ) ;
#11285 = CARTESIAN_POINT ( 'NONE',  ( -16.39856880423293006, -20.52544743201270450, 56.85231026484400019 ) ) ;
#11287 = EDGE_LOOP ( 'NONE', ( #3981, #11557 ) ) ;
#11288 = CARTESIAN_POINT ( 'NONE',  ( -24.93814746875458610, -16.73481322911949931, 56.85231026484398598 ) ) ;
#11289 = CYLINDRICAL_SURFACE ( 'NONE', #14141, 10.00000000000000000 ) ;
#11290 = VERTEX_POINT ( 'NONE', #11642 ) ;
#11291 = FACE_OUTER_BOUND ( 'NONE', #5294, .T. ) ;
#11292 = ADVANCED_FACE ( 'NONE', ( #6734, #10419, #6814, #1089 ), #8040, .T. ) ;
#11293 = VECTOR ( 'NONE', #6980, 1000.000000000000114 ) ;
#11294 = CARTESIAN_POINT ( 'NONE',  ( -18.07633053687676750, -36.92914190242253625, -17.90990850420651626 ) ) ;
#11295 = VECTOR ( 'NONE', #12855, 1000.000000000000000 ) ;
#11296 = ORIENTED_EDGE ( 'NONE', *, *, #6675, .F. ) ;
#11297 = CARTESIAN_POINT ( 'NONE',  ( -35.18530787408279537, 11.99262100756689620, 16.16206422150100153 ) ) ;
#11298 = AXIS2_PLACEMENT_3D ( 'NONE', #5180, #300, #10854 ) ;
#11299 = DIRECTION ( 'NONE',  ( 1.445602896647337931E-16, 0.000000000000000000, -1.000000000000000000 ) ) ;
#11300 = ITEM_DEFINED_TRANSFORMATION ( 'NONE', 'NONE', #4625,  #6789 ) ;
#11301 = DIRECTION ( 'NONE',  ( -0.3633925226508256667, 0.9316361277244830097, -8.480480961564259036E-16 ) ) ;
#11302 = CIRCLE ( 'NONE', #6646, 1.600959456836780204 ) ;
#11303 = CIRCLE ( 'NONE', #10070, 22.99999999999999645 ) ;
#11304 = CARTESIAN_POINT ( 'NONE',  ( -15.51120972694785749, -13.45872179377749589, 56.85231026484398598 ) ) ;
#11305 = EDGE_CURVE ( 'NONE', #777, #9604, #1741, .T. ) ;
#11306 = DIRECTION ( 'NONE',  ( -1.000000000000000000, -1.000000000000000078E-15, -1.000000000000000078E-15 ) ) ;
#11307 = ORIENTED_EDGE ( 'NONE', *, *, #706, .F. ) ;
#11308 = CARTESIAN_POINT ( 'NONE',  ( -24.06473463808513813, -13.92741382918746496, 56.85231026484398598 ) ) ;
#11309 = EDGE_CURVE ( 'NONE', #14890, #6515, #13982, .T. ) ;
#11310 = CARTESIAN_POINT ( 'NONE',  ( -7.508831348196946642, -44.91519662196459706, -3.570265637683905702 ) ) ;
#11311 = EDGE_CURVE ( 'NONE', #7355, #13071, #2998, .T. ) ;
#11312 = ORIENTED_EDGE ( 'NONE', *, *, #12608, .F. ) ;
#11313 = ORIENTED_EDGE ( 'NONE', *, *, #7785, .F. ) ;
#11314 = ORIENTED_EDGE ( 'NONE', *, *, #10633, .T. ) ;
#11315 = CARTESIAN_POINT ( 'NONE',  ( -7.754798889200088752, -46.50763646577239285, -7.996864293225370623 ) ) ;
#11316 = CARTESIAN_POINT ( 'NONE',  ( -15.21745595230144232, -22.57829892241827352, 56.85231026484400019 ) ) ;
#11317 = ADVANCED_FACE ( 'NONE', ( #4387 ), #9040, .F. ) ;
#11318 = CIRCLE ( 'NONE', #2516, 37.50000000000000000 ) ;
#11320 = AXIS2_PLACEMENT_3D ( 'NONE', #2337, #11588, #1105 ) ;
#11319 = DIRECTION ( 'NONE',  ( 0.9472588896649092316, -0.3204693369899889732, 9.510565162951523791E-16 ) ) ;
#11321 = DIRECTION ( 'NONE',  ( -8.018662683283438208E-16, 5.975035461963189015E-16, 1.000000000000000000 ) ) ;
#11322 = CARTESIAN_POINT ( 'NONE',  ( -5.519619651378201652, -12.85420092285971805, 60.35966704321151610 ) ) ;
#11323 = CARTESIAN_POINT ( 'NONE',  ( -17.81448839017816965, -11.78253482624722182, 56.75231026484397745 ) ) ;
#11324 = EDGE_CURVE ( 'NONE', #14274, #9541, #7346, .T. ) ;
#11325 = CARTESIAN_POINT ( 'NONE',  ( -35.49969986081099904, -19.50737899243800300, -123.9247733198440073 ) ) ;
#11326 = AXIS2_PLACEMENT_3D ( 'NONE', #3662, #9622, #6013 ) ;
#11327 = LINE ( 'NONE', #14844, #12533 ) ;
#11328 = EDGE_LOOP ( 'NONE', ( #2773, #5608, #2717, #9428 ) ) ;
#11329 = CARTESIAN_POINT ( 'NONE',  ( -5.966797098401854349, -16.44411015522000241, 57.00231026484399166 ) ) ;
#11330 = ORIENTED_EDGE ( 'NONE', *, *, #11900, .F. ) ;
#11331 = DIRECTION ( 'NONE',  ( 0.000000000000000000, 0.1872998510044689147, 0.9823027872370635460 ) ) ;
#11333 = VERTEX_POINT ( 'NONE', #3615 ) ;
#11332 = CARTESIAN_POINT ( 'NONE',  ( -24.60545001190342873, -9.363048095758424338, 60.58996776729609479 ) ) ;
#11334 = ORIENTED_EDGE ( 'NONE', *, *, #1501, .T. ) ;
#11335 =( REPRESENTATION_RELATIONSHIP ('NONE','NONE', #2372, #3931 ) REPRESENTATION_RELATIONSHIP_WITH_TRANSFORMATION ( #9149 )SHAPE_REPRESENTATION_RELATIONSHIP( ) );
#11336 = CARTESIAN_POINT ( 'NONE',  ( -20.65541546412893226, -22.04665423204159325, 54.00231026484399166 ) ) ;
#11337 = ORIENTED_EDGE ( 'NONE', *, *, #1952, .T. ) ;
#11338 = LINE ( 'NONE', #6727, #6079 ) ;
#11339 = CARTESIAN_POINT ( 'NONE',  ( -23.49969986081099904, -44.50737899243799944, -109.5506571639849938 ) ) ;
#11340 = ADVANCED_FACE ( 'NONE', ( #4997 ), #12029, .F. ) ;
#11341 = VECTOR ( 'NONE', #8297, 1000.000000000000000 ) ;
#11342 = CARTESIAN_POINT ( 'NONE',  ( -18.09969986081099336, -109.4641865893815407, -10.25678343939419968 ) ) ;
#11343 =( BOUNDED_CURVE ( )  B_SPLINE_CURVE ( 3, ( #3438, #4666, #156, #13998 ),
 .UNSPECIFIED., .F., .F. ) 
 B_SPLINE_CURVE_WITH_KNOTS ( ( 4, 4 ),
 ( 3.141592653589792228, 4.712388980384688786 ),
 .UNSPECIFIED. ) 
 CURVE ( )  GEOMETRIC_REPRESENTATION_ITEM ( )  RATIONAL_B_SPLINE_CURVE ( ( 1.000000000000000000, 0.8047378541243649375, 0.8047378541243649375, 1.000000000000000000 ) ) 
 REPRESENTATION_ITEM ( '' )  );
#11344 = CARTESIAN_POINT ( 'NONE',  ( -6.517576446443361426, -14.80457171870128974, 56.85231026484400019 ) ) ;
#11345 = AXIS2_PLACEMENT_3D ( 'NONE', #6214, #1562, #6062 ) ;
#11346 = CARTESIAN_POINT ( 'NONE',  ( -34.99969986081099904, -20.37340439622244048, -12.52892449124999885 ) ) ;
#11347 = ORIENTED_EDGE ( 'NONE', *, *, #3938, .T. ) ;
#11348 = CARTESIAN_POINT ( 'NONE',  ( 15.51479836175852789, -24.50194921392514757, 45.29248735876494436 ) ) ;
#11349 = ORIENTED_EDGE ( 'NONE', *, *, #2708, .F. ) ;
#11350 = LINE ( 'NONE', #3245, #10677 ) ;
#11351 = ORIENTED_EDGE ( 'NONE', *, *, #2573, .F. ) ;
#11352 = ORIENTED_EDGE ( 'NONE', *, *, #159, .T. ) ;
#11353 = AXIS2_PLACEMENT_3D ( 'NONE', #5245, #6522, #7605 ) ;
#11354 = FACE_OUTER_BOUND ( 'NONE', #12634, .T. ) ;
#11355 = VERTEX_POINT ( 'NONE', #10575 ) ;
#11356 = CARTESIAN_POINT ( 'NONE',  ( -7.499699860810998153, -44.50737899243799944, 56.13904046828873362 ) ) ;
#11357 = EDGE_CURVE ( 'NONE', #3429, #9206, #10729, .T. ) ;
#11358 = FACE_OUTER_BOUND ( 'NONE', #14060, .T. ) ;
#11359 = DIRECTION ( 'NONE',  ( -1.000000000000000000, 0.000000000000000000, -1.011922027653137143E-15 ) ) ;
#11360 = CIRCLE ( 'NONE', #7200, 8.000000000000000000 ) ;
#11361 = CARTESIAN_POINT ( 'NONE',  ( 14.95706336429091721, -25.48138479685667690, 2.334038900917459358 ) ) ;
#11362 = CYLINDRICAL_SURFACE ( 'NONE', #111, 2.500000000000000000 ) ;
#11364 = DIRECTION ( 'NONE',  ( 0.000000000000000000, 1.000000000000000000, 1.224646799147350002E-16 ) ) ;
#11363 = DIRECTION ( 'NONE',  ( 0.000000000000000000, 0.000000000000000000, -1.000000000000000000 ) ) ;
#11365 = ORIENTED_EDGE ( 'NONE', *, *, #9404, .F. ) ;
#11366 = CARTESIAN_POINT ( 'NONE',  ( -11.90127153857800657, -52.50737899243802786, 2.502310264844031185 ) ) ;
#11367 = DIRECTION ( 'NONE',  ( -8.660254037844387408E-16, 0.8660254037844387076, -0.4999999999999998890 ) ) ;
#11368 = ORIENTED_EDGE ( 'NONE', *, *, #2386, .T. ) ;
#11369 = VERTEX_POINT ( 'NONE', #8348 ) ;
#11370 = DIRECTION ( 'NONE',  ( 0.000000000000000000, -1.000000000000000000, -1.224646799147350002E-16 ) ) ;
#11371 = DIRECTION ( 'NONE',  ( 8.018662683283438208E-16, -5.975035461963189015E-16, -1.000000000000000000 ) ) ;
#11372 = CARTESIAN_POINT ( 'NONE',  ( -17.54761070396351741, -21.31837676343380750, 56.85231026484400019 ) ) ;
#11373 = ORIENTED_EDGE ( 'NONE', *, *, #10588, .F. ) ;
#11374 = DIRECTION ( 'NONE',  ( 0.000000000000000000, 0.000000000000000000, 1.000000000000000000 ) ) ;
#11375 = EDGE_CURVE ( 'NONE', #8725, #5040, #13110, .T. ) ;
#11376 = DIRECTION ( 'NONE',  ( 8.018662683283438208E-16, -5.975035461963189015E-16, -1.000000000000000000 ) ) ;
#11377 = CARTESIAN_POINT ( 'NONE',  ( -23.59767874945767119, -17.60420555931063902, 57.00231026484397745 ) ) ;
#11378 = CARTESIAN_POINT ( 'NONE',  ( -17.54761070396351741, -21.31837676343380750, 56.85231026484400019 ) ) ;
#11379 = DIRECTION ( 'NONE',  ( 0.3533329742249663452, 0.9354976265738675911, -2.756373558169968730E-16 ) ) ;
#11380 = VECTOR ( 'NONE', #799, 1000.000000000000000 ) ;
#11381 = EDGE_LOOP ( 'NONE', ( #3809, #14256, #14182, #4069 ) ) ;
#11382 = CARTESIAN_POINT ( 'NONE',  ( -11.44122778921134120, -90.82924336192752435, -1.978697273178005034 ) ) ;
#11383 = CARTESIAN_POINT ( 'NONE',  ( -7.503594565398491234, -44.64029237675795514, -3.819848327953776934 ) ) ;
#11384 = ORIENTED_EDGE ( 'NONE', *, *, #5632, .T. ) ;
#11386 = ORIENTED_EDGE ( 'NONE', *, *, #1417, .F. ) ;
#11385 = CARTESIAN_POINT ( 'NONE',  ( -15.57469986081099478, -23.50737899243800300, 56.85231026484400019 ) ) ;
#11387 = ORIENTED_EDGE ( 'NONE', *, *, #11908, .T. ) ;
#11388 = CARTESIAN_POINT ( 'NONE',  ( -15.49969986081092088, -13.50737899243822504, 56.85231026484398598 ) ) ;
#11389 = CARTESIAN_POINT ( 'NONE',  ( -10.02446058099324766, -7.572113216692248017, 57.00231026484397745 ) ) ;
#11390 = ADVANCED_FACE ( 'NONE', ( #1323 ), #3692, .T. ) ;
#11391 = CARTESIAN_POINT ( 'NONE',  ( -12.91190996461674168, -5.858263458394094236, 56.85231026484398598 ) ) ;
#11392 = LINE ( 'NONE', #7639, #10124 ) ;
#11393 = CIRCLE ( 'NONE', #14329, 9.974999999999999645 ) ;
#11394 = EDGE_CURVE ( 'NONE', #7739, #1092, #9501, .T. ) ;
#11395 = CARTESIAN_POINT ( 'NONE',  ( -21.05979293892203330, -6.334749421441233430, 57.00231026484397745 ) ) ;
#11396 = DIRECTION ( 'NONE',  ( -0.5975035461963188466, -0.8018662683283439563, 0.000000000000000000 ) ) ;
#11397 = CARTESIAN_POINT ( 'NONE',  ( 4.500300139189000959, -19.50737899243801010, -123.9247733198440073 ) ) ;
#11398 = ADVANCED_FACE ( 'NONE', ( #2693 ), #12048, .T. ) ;
#11399 = CARTESIAN_POINT ( 'NONE',  ( -23.54290256004220439, -7.607589560680598773, 56.85231026484398598 ) ) ;
#11400 = ORIENTED_EDGE ( 'NONE', *, *, #14106, .T. ) ;
#11401 = CARTESIAN_POINT ( 'NONE',  ( 14.77482671525745594, -27.91392081745070897, 46.34137906563161380 ) ) ;
#11402 = VECTOR ( 'NONE', #7011, 1000.000000000000000 ) ;
#11403 = ORIENTED_EDGE ( 'NONE', *, *, #11866, .F. ) ;
#11405 = ORIENTED_EDGE ( 'NONE', *, *, #4296, .T. ) ;
#11404 = CARTESIAN_POINT ( 'NONE',  ( -8.972439834930606040, -10.77678811232731348, 57.00231026484399166 ) ) ;
#11406 = ORIENTED_EDGE ( 'NONE', *, *, #1603, .F. ) ;
#11407 = PLANE ( 'NONE',  #9945 ) ;
#11408 = ORIENTED_EDGE ( 'NONE', *, *, #13881, .F. ) ;
#11409 = AXIS2_PLACEMENT_3D ( 'NONE', #8898, #3085, #8742 ) ;
#11410 = CARTESIAN_POINT ( 'NONE',  ( -15.54961651457173488, -13.51026476396819831, 56.85231026484398598 ) ) ;
#11411 = EDGE_CURVE ( 'NONE', #9329, #6799, #8194, .T. ) ;
#11412 = ADVANCED_FACE ( 'NONE', ( #8270 ), #1546, .F. ) ;
#11413 = AXIS2_PLACEMENT_3D ( 'NONE', #9769, #9540, #5107 ) ;
#11414 = DIRECTION ( 'NONE',  ( 0.000000000000000000, -1.224646799147350002E-16, 1.000000000000000000 ) ) ;
#11415 = DIRECTION ( 'NONE',  ( -0.4587843131450204948, 0.8885476655824671166, -8.987940462991649850E-16 ) ) ;
#11416 = VECTOR ( 'NONE', #11934, 1000.000000000000000 ) ;
#11417 = ORIENTED_EDGE ( 'NONE', *, *, #1537, .F. ) ;
#11418 = DIRECTION ( 'NONE',  ( 0.8357240892757724637, 0.5491495666976171641, 3.420201433256690644E-16 ) ) ;
#11419 = CARTESIAN_POINT ( 'NONE',  ( -22.78941651591205186, -47.81319948894917360, -17.28247564077643261 ) ) ;
#11420 = VERTEX_POINT ( 'NONE', #6200 ) ;
#11421 = FACE_OUTER_BOUND ( 'NONE', #11145, .T. ) ;
#11422 = VERTEX_POINT ( 'NONE', #5977 ) ;
#11423 = PLANE ( 'NONE',  #10178 ) ;
#11424 = ORIENTED_EDGE ( 'NONE', *, *, #13542, .T. ) ;
#11425 = EDGE_LOOP ( 'NONE', ( #6498, #5676, #3922, #4336 ) ) ;
#11426 = B_SPLINE_CURVE_WITH_KNOTS ( 'NONE', 3,
 ( #3216, #3058, #2785, #11176, #14843, #12117, #7791, #10092 ),
 .UNSPECIFIED., .F., .F.,
 ( 4, 2, 2, 4 ),
 ( 0.000000000000000000, 0.2499999999999999445, 0.4999999999999998890, 1.000000000000000000 ),
 .UNSPECIFIED. ) ;
#11427 = DIRECTION ( 'NONE',  ( 1.000000000000000000, -1.291538348938060198E-32, 1.054621095516909827E-16 ) ) ;
#11428 = VERTEX_POINT ( 'NONE', #12881 ) ;
#11429 = AXIS2_PLACEMENT_3D ( 'NONE', #1416, #10518, #5916 ) ;
#11430 = CARTESIAN_POINT ( 'NONE',  ( -7.909388035719858934, -41.92610292194794397, 56.22667989926442544 ) ) ;
#11431 = ADVANCED_FACE ( 'NONE', ( #6045 ), #7038, .F. ) ;
#11432 = CARTESIAN_POINT ( 'NONE',  ( -10.59381597806627795, -90.60492159835612824, -7.685054528635899551 ) ) ;
#11433 = VECTOR ( 'NONE', #6867, 1000.000000000000000 ) ;
#11434 = FACE_OUTER_BOUND ( 'NONE', #6123, .T. ) ;
#11436 = CARTESIAN_POINT ( 'NONE',  ( -15.49969986081099727, 22.99262100756199700, 39.83706422150100224 ) ) ;
#11435 = FACE_OUTER_BOUND ( 'NONE', #3621, .T. ) ;
#11437 = VERTEX_POINT ( 'NONE', #10882 ) ;
#11438 = DIRECTION ( 'NONE',  ( 0.000000000000000000, 1.000000000000000000, 1.224646799147350002E-16 ) ) ;
#11439 = CARTESIAN_POINT ( 'NONE',  ( -19.99969986081099549, -13.80506132690247512, -13.01695671647155095 ) ) ;
#11440 = ORIENTED_EDGE ( 'NONE', *, *, #8527, .T. ) ;
#11441 = ORIENTED_EDGE ( 'NONE', *, *, #8537, .F. ) ;
#11442 = FACE_OUTER_BOUND ( 'NONE', #4604, .T. ) ;
#11443 = EDGE_CURVE ( 'NONE', #8638, #9137, #7145, .T. ) ;
#11444 = DIRECTION ( 'NONE',  ( 0.000000000000000000, 0.000000000000000000, -1.000000000000000000 ) ) ;
#11445 = CARTESIAN_POINT ( 'NONE',  ( -15.97834026492444437, -93.97082955884093280, -10.96837812141254354 ) ) ;
#11446 = ORIENTED_EDGE ( 'NONE', *, *, #1666, .F. ) ;
#11447 = FACE_OUTER_BOUND ( 'NONE', #6491, .T. ) ;
#11448 = AXIS2_PLACEMENT_3D ( 'NONE', #6291, #14413, #9745 ) ;
#11449 = VECTOR ( 'NONE', #5396, 1000.000000000000000 ) ;
#11450 = AXIS2_PLACEMENT_3D ( 'NONE', #10593, #13054, #12899 ) ;
#11451 = CARTESIAN_POINT ( 'NONE',  ( -15.49969986081099727, 70.89785811302749607, 33.09844592272734332 ) ) ;
#11452 = CONTEXT_DEPENDENT_SHAPE_REPRESENTATION ( #9772, #9939 ) ;
#11453 = CARTESIAN_POINT ( 'NONE',  ( -15.61203582816999891, -106.7406604375499626, -7.297873098422156701 ) ) ;
#11454 = AXIS2_PLACEMENT_3D ( 'NONE', #6120, #13339, #5140 ) ;
#11455 = PLANE ( 'NONE',  #6238 ) ;
#11456 = CARTESIAN_POINT ( 'NONE',  ( -2.216578225681298697, -32.00737899243799944, -10.85656391856669778 ) ) ;
#11457 = ORIENTED_EDGE ( 'NONE', *, *, #5391, .F. ) ;
#11458 = CARTESIAN_POINT ( 'NONE',  ( -15.26264886222055139, -94.81047857984601990, -0.1311698051623074457 ) ) ;
#11459 = DIRECTION ( 'NONE',  ( 0.4800904676395346127, 0.8772189822852974883, -1.391731009600680140E-16 ) ) ;
#11460 = CARTESIAN_POINT ( 'NONE',  ( -15.49969986081092088, -13.50737899243822504, 57.00231026484397745 ) ) ;
#11461 = EDGE_CURVE ( 'NONE', #8254, #12986, #11872, .T. ) ;
#11462 = DIRECTION ( 'NONE',  ( 0.000000000000000000, 0.000000000000000000, 1.000000000000000000 ) ) ;
#11463 = VERTEX_POINT ( 'NONE', #8426 ) ;
#11464 = CARTESIAN_POINT ( 'NONE',  ( -15.12969879992303746, -10.35358246313022335, 57.00231026484397745 ) ) ;
#11465 = EDGE_LOOP ( 'NONE', ( #3263, #14419, #14449, #12145 ) ) ;
#11466 = CARTESIAN_POINT ( 'NONE',  ( -13.26502611401716081, -13.76954925274777253, 51.00231026484399166 ) ) ;
#11467 = CARTESIAN_POINT ( 'NONE',  ( -15.49969986081091378, -13.50737899243822859, 51.00231026484399166 ) ) ;
#11468 = VECTOR ( 'NONE', #14410, 1000.000000000000000 ) ;
#11469 = AXIS2_PLACEMENT_3D ( 'NONE', #8458, #4798, #5928 ) ;
#11470 = CYLINDRICAL_SURFACE ( 'NONE', #1033, 2.499999999999998668 ) ;
#11471 = CARTESIAN_POINT ( 'NONE',  ( 9.000300139189000959, -32.00737899243799944, 52.60220335465780295 ) ) ;
#11472 = DIRECTION ( 'NONE',  ( 1.000000000000000000, 1.201369187114119994E-15, 9.616040805000176517E-16 ) ) ;
#11473 = CARTESIAN_POINT ( 'NONE',  ( -14.61203582817000068, -106.6563755045979605, -6.855836844165474453 ) ) ;
#11474 = CARTESIAN_POINT ( 'NONE',  ( -15.49969986081100437, -104.2799573210345869, -4.173688775771633885 ) ) ;
#11475 = CARTESIAN_POINT ( 'NONE',  ( -23.41792317787242084, -15.09084496969942535, 56.85231026484398598 ) ) ;
#11476 = ADVANCED_FACE ( 'NONE', ( #2617 ), #6652, .T. ) ;
#11477 = VERTEX_POINT ( 'NONE', #407 ) ;
#11478 = CARTESIAN_POINT ( 'NONE',  ( 14.68618260102869932, -27.00737899243800300, 46.46206422150099513 ) ) ;
#11479 = ORIENTED_EDGE ( 'NONE', *, *, #13016, .T. ) ;
#11480 = CARTESIAN_POINT ( 'NONE',  ( -17.62015867087677634, -21.29935591968936137, 56.85231026484400019 ) ) ;
#11482 = ORIENTED_EDGE ( 'NONE', *, *, #8312, .T. ) ;
#11481 = LINE ( 'NONE', #1999, #13768 ) ;
#11483 = ORIENTED_EDGE ( 'NONE', *, *, #1407, .T. ) ;
#11484 = EDGE_CURVE ( 'NONE', #10814, #12333, #11303, .T. ) ;
#11485 = AXIS2_PLACEMENT_3D ( 'NONE', #4004, #11115, #5081 ) ;
#11486 = CARTESIAN_POINT ( 'NONE',  ( -10.95221305062249684, -4.629260458021021485, 57.00231026484397745 ) ) ;
#11487 = ORIENTED_EDGE ( 'NONE', *, *, #11952, .T. ) ;
#11488 = CARTESIAN_POINT ( 'NONE',  ( -15.61203582817000068, -106.4047424672253186, -6.741402868119606318 ) ) ;
#11489 = LINE ( 'NONE', #12725, #2946 ) ;
#11490 =( NAMED_UNIT ( * ) PLANE_ANGLE_UNIT ( ) SI_UNIT ( $, .RADIAN. ) );
#11491 = ORIENTED_EDGE ( 'NONE', *, *, #12396, .T. ) ;
#11492 = CARTESIAN_POINT ( 'NONE',  ( 9.000300139189000959, -19.50737899243800300, 24.21206422150099868 ) ) ;
#11493 = ADVANCED_FACE ( 'NONE', ( #548 ), #1845, .T. ) ;
#11494 = ORIENTED_EDGE ( 'NONE', *, *, #10282, .F. ) ;
#11495 = CARTESIAN_POINT ( 'NONE',  ( 14.68618260102869577, -26.77367873612697480, 46.46206422150098803 ) ) ;
#11496 = EDGE_CURVE ( 'NONE', #5981, #10261, #11743, .T. ) ;
#11497 = EDGE_LOOP ( 'NONE', ( #7587, #15114 ) ) ;
#11498 = CARTESIAN_POINT ( 'NONE',  ( -5.499699860811000818, -46.50737899243799944, 19.50231026484399877 ) ) ;
#11499 = ORIENTED_EDGE ( 'NONE', *, *, #9923, .F. ) ;
#11500 = ORIENTED_EDGE ( 'NONE', *, *, #7905, .T. ) ;
#11501 = DIRECTION ( 'NONE',  ( 1.000000000000000000, 1.000000000000000078E-15, 1.000000000000000078E-15 ) ) ;
#11502 = ORIENTED_EDGE ( 'NONE', *, *, #1632, .T. ) ;
#11503 = CARTESIAN_POINT ( 'NONE',  ( -7.512805849530849400, -44.04964101872660365, 19.96004823855532706 ) ) ;
#11504 = EDGE_CURVE ( 'NONE', #2864, #1781, #12105, .T. ) ;
#11505 = DIRECTION ( 'NONE',  ( 0.9316361277244830097, 0.3633925226508256667, 5.299192642332049884E-16 ) ) ;
#11506 = DIRECTION ( 'NONE',  ( 0.000000000000000000, 1.850371707708594316E-16, -1.000000000000000000 ) ) ;
#11507 = VECTOR ( 'NONE', #3158, 1000.000000000000000 ) ;
#11508 = DIRECTION ( 'NONE',  ( -1.734723475976807094E-16, 0.000000000000000000, 1.000000000000000000 ) ) ;
#11510 = CARTESIAN_POINT ( 'NONE',  ( -15.49969986081099904, 71.39262100756199914, 24.21206422150100579 ) ) ;
#11509 = DIRECTION ( 'NONE',  ( 0.5975035461963188466, 0.8018662683283437342, 0.000000000000000000 ) ) ;
#11511 = ORIENTED_EDGE ( 'NONE', *, *, #7971, .T. ) ;
#11512 = DIRECTION ( 'NONE',  ( -8.018662683283438208E-16, 5.975035461963189015E-16, 1.000000000000000000 ) ) ;
#11513 = EDGE_CURVE ( 'NONE', #1909, #13227, #1767, .T. ) ;
#11514 = EDGE_CURVE ( 'NONE', #4715, #9010, #13260, .T. ) ;
#11515 = LINE ( 'NONE', #12750, #7883 ) ;
#11516 = ORIENTED_EDGE ( 'NONE', *, *, #5445, .F. ) ;
#11517 = CARTESIAN_POINT ( 'NONE',  ( -14.76203582817000104, -107.1622034095870077, -6.087689735155999315 ) ) ;
#11518 = ADVANCED_FACE ( 'NONE', ( #4142 ), #6347, .T. ) ;
#11519 = LINE ( 'NONE', #893, #3968 ) ;
#11520 = CARTESIAN_POINT ( 'NONE',  ( -24.03943920472178775, -16.57887731378902885, 56.85231026484398598 ) ) ;
#11521 = ORIENTED_EDGE ( 'NONE', *, *, #3746, .F. ) ;
#11522 = FACE_OUTER_BOUND ( 'NONE', #8948, .T. ) ;
#11523 = CIRCLE ( 'NONE', #1253, 9.974999999999999645 ) ;
#11524 = CARTESIAN_POINT ( 'NONE',  ( -14.61203582817000068, -106.7406604375499626, -7.297873098422155813 ) ) ;
#11525 = PRODUCT_DEFINITION ( 'UNKNOWN', '', #3893, #4830 ) ;
#11526 = EDGE_CURVE ( 'NONE', #6877, #2831, #4063, .T. ) ;
#11527 = DIRECTION ( 'NONE',  ( 0.000000000000000000, 0.1872998510044689147, 0.9823027872370635460 ) ) ;
#11528 = DIRECTION ( 'NONE',  ( 0.5975035461963189576, 0.8018662683283437342, 0.000000000000000000 ) ) ;
#11529 = CARTESIAN_POINT ( 'NONE',  ( -5.499699860810998153, -46.50737899243799944, -5.497689735156003010 ) ) ;
#11530 =( REPRESENTATION_RELATIONSHIP ('NONE','NONE', #2372, #3931 ) REPRESENTATION_RELATIONSHIP_WITH_TRANSFORMATION ( #2354 )SHAPE_REPRESENTATION_RELATIONSHIP( ) );
#11531 = AXIS2_PLACEMENT_3D ( 'NONE', #10041, #11427, #13652 ) ;
#11532 = ORIENTED_EDGE ( 'NONE', *, *, #4947, .F. ) ;
#11533 = CARTESIAN_POINT ( 'NONE',  ( -11.24943535381201087, -90.76549582974007535, -2.207202805067481677 ) ) ;
#11534 = VECTOR ( 'NONE', #10541, 1000.000000000000000 ) ;
#11535 = CARTESIAN_POINT ( 'NONE',  ( -10.90377457632059865, -6.867868786151726468, 56.85231026484398598 ) ) ;
#11536 = CARTESIAN_POINT ( 'NONE',  ( -15.49969986081099194, -27.00737899243800300, 19.50231026484399877 ) ) ;
#11537 = VECTOR ( 'NONE', #1927, 1000.000000000000114 ) ;
#11538 = AXIS2_PLACEMENT_3D ( 'NONE', #15125, #6936, #11545 ) ;
#11539 = LINE ( 'NONE', #15054, #10227 ) ;
#11540 = EDGE_LOOP ( 'NONE', ( #8008, #8683, #10772, #2090, #14865 ) ) ;
#11541 = CARTESIAN_POINT ( 'NONE',  ( -7.490307934913750465, -12.48011759562962020, 56.85231026484400019 ) ) ;
#11542 = VERTEX_POINT ( 'NONE', #6490 ) ;
#11543 = CARTESIAN_POINT ( 'NONE',  ( -7.887638505697306179, -19.95386229157006497, 57.00231026484399166 ) ) ;
#11544 = LINE ( 'NONE', #7082, #685 ) ;
#11545 = DIRECTION ( 'NONE',  ( 0.5975035461963188466, 0.8018662683283437342, 0.000000000000000000 ) ) ;
#11546 = CARTESIAN_POINT ( 'NONE',  ( -3.508527451665000463, -45.64135358865355840, -6.997689735156000346 ) ) ;
#11547 = VECTOR ( 'NONE', #12390, 1000.000000000000000 ) ;
#11548 = EDGE_CURVE ( 'NONE', #12614, #1349, #11021, .T. ) ;
#11549 = AXIS2_PLACEMENT_3D ( 'NONE', #5361, #10018, #7715 ) ;
#11550 = DIRECTION ( 'NONE',  ( 0.000000000000000000, 0.000000000000000000, -1.000000000000000000 ) ) ;
#11551 = CARTESIAN_POINT ( 'NONE',  ( -15.24029490235350259, -21.57855976525750563, 56.85231026484400019 ) ) ;
#11552 = LINE ( 'NONE', #2221, #4114 ) ;
#11553 = LINE ( 'NONE', #7866, #3491 ) ;
#11554 = ORIENTED_EDGE ( 'NONE', *, *, #14784, .T. ) ;
#11555 = DIRECTION ( 'NONE',  ( 0.5975035461963189576, 0.8018662683283437342, 0.000000000000000000 ) ) ;
#11556 = PRODUCT_DEFINITION_CONTEXT ( 'detailed design', #8688, 'design' ) ;
#11557 = ORIENTED_EDGE ( 'NONE', *, *, #942, .F. ) ;
#11559 = ORIENTED_EDGE ( 'NONE', *, *, #11900, .T. ) ;
#11558 = CARTESIAN_POINT ( 'NONE',  ( -25.49738368519668086, -13.18106784639022244, 60.35478574090821269 ) ) ;
#11560 = ORIENTED_EDGE ( 'NONE', *, *, #7482, .F. ) ;
#11561 = CARTESIAN_POINT ( 'NONE',  ( -18.09969986081100046, -107.1622034095870077, -6.087689735156001980 ) ) ;
#11562 = PLANE ( 'NONE',  #4349 ) ;
#11563 = AXIS2_PLACEMENT_3D ( 'NONE', #43, #13887, #8055 ) ;
#11564 = ORIENTED_EDGE ( 'NONE', *, *, #12788, .F. ) ;
#11565 = DIRECTION ( 'NONE',  ( 0.000000000000000000, -1.000000000000000000, -1.224646799147350002E-16 ) ) ;
#11566 = ADVANCED_FACE ( 'NONE', ( #7500, #10957, #1922 ), #14547, .T. ) ;
#11567 = DIRECTION ( 'NONE',  ( 1.000000000000000000, -1.291538348938060198E-32, 1.054621095516909827E-16 ) ) ;
#11568 = CIRCLE ( 'NONE', #14018, 2.499999999999998668 ) ;
#11569 = EDGE_CURVE ( 'NONE', #13213, #6631, #12705, .T. ) ;
#11570 = CARTESIAN_POINT ( 'NONE',  ( -22.29355530218780501, -48.73954551910809840, -17.37742864379163876 ) ) ;
#11571 = EDGE_LOOP ( 'NONE', ( #13858, #13480, #949, #7443 ) ) ;
#11572 = CARTESIAN_POINT ( 'NONE',  ( 15.84905121855136478, -24.16036003417319122, 44.79232149582683320 ) ) ;
#11573 = ORIENTED_EDGE ( 'NONE', *, *, #12456, .T. ) ;
#11574 = AXIS2_PLACEMENT_3D ( 'NONE', #6598, #14655, #7756 ) ;
#11575 = ORIENTED_EDGE ( 'NONE', *, *, #6093, .T. ) ;
#11576 = ORIENTED_EDGE ( 'NONE', *, *, #10466, .T. ) ;
#11577 = CARTESIAN_POINT ( 'NONE',  ( 2.510125670910141160, -41.64595657060088740, 52.39450821273811698 ) ) ;
#11578 = ORIENTED_EDGE ( 'NONE', *, *, #8138, .F. ) ;
#11579 = CARTESIAN_POINT ( 'NONE',  ( -20.85440823583763859, -21.95508377545333900, 56.61960193865294144 ) ) ;
#11580 = EDGE_CURVE ( 'NONE', #3001, #970, #4226, .T. ) ;
#11581 = DIRECTION ( 'NONE',  ( 0.000000000000000000, -1.000000000000000000, -1.224646799147350002E-16 ) ) ;
#11582 = LINE ( 'NONE', #10204, #8263 ) ;
#11583 = ADVANCED_FACE ( 'NONE', ( #772 ), #14693, .F. ) ;
#11584 = AXIS2_PLACEMENT_3D ( 'NONE', #12975, #5013, #13205 ) ;
#11585 = EDGE_CURVE ( 'NONE', #11857, #4102, #13926, .T. ) ;
#11586 = VECTOR ( 'NONE', #4572, 1000.000000000000114 ) ;
#11587 = CARTESIAN_POINT ( 'NONE',  ( -6.468284635389320414, -17.74225372801456757, 56.85231026484400019 ) ) ;
#11589 = DIRECTION ( 'NONE',  ( -8.018662683283438208E-16, 5.975035461963189015E-16, 1.000000000000000000 ) ) ;
#11588 = DIRECTION ( 'NONE',  ( -1.000000000000000000, -1.201369187114119994E-15, -9.616040805000176517E-16 ) ) ;
#11590 = EDGE_LOOP ( 'NONE', ( #1472, #2111, #704, #13307 ) ) ;
#11591 = CARTESIAN_POINT ( 'NONE',  ( -7.568963286690253867, -45.57243725087103314, 42.17552517324416783 ) ) ;
#11592 = CARTESIAN_POINT ( 'NONE',  ( -15.49969986081099904, 20.99262100756200056, 24.21206422150099868 ) ) ;
#11593 = ORIENTED_EDGE ( 'NONE', *, *, #3386, .T. ) ;
#11594 = EDGE_CURVE ( 'NONE', #7160, #7645, #9249, .T. ) ;
#11595 = VERTEX_POINT ( 'NONE', #3217 ) ;
#11596 = DIRECTION ( 'NONE',  ( 1.000000000000000000, 1.201369187114119994E-15, 9.616040805000176517E-16 ) ) ;
#11597 = DIRECTION ( 'NONE',  ( 0.9316361277244821215, 0.3633925226508276651, 5.299192642332029177E-16 ) ) ;
#11598 = EDGE_LOOP ( 'NONE', ( #5719, #3775, #9948, #13793 ) ) ;
#11599 = LINE ( 'NONE', #1116, #12012 ) ;
#11600 = ADVANCED_FACE ( 'NONE', ( #5508 ), #3441, .F. ) ;
#11601 = AXIS2_PLACEMENT_3D ( 'NONE', #14947, #1102, #6899 ) ;
#11602 = EDGE_CURVE ( 'NONE', #551, #6428, #11553, .T. ) ;
#11603 = DIRECTION ( 'NONE',  ( 0.5104125104778984845, 0.8599296884906632021, -1.045284632676530333E-16 ) ) ;
#11604 = ADVANCED_FACE ( 'NONE', ( #2075 ), #13625, .F. ) ;
#11605 = DIRECTION ( 'NONE',  ( -0.9918751611018171710, -0.1272150336605082366, -7.193398003386512876E-16 ) ) ;
#11606 = DIRECTION ( 'NONE',  ( -3.202566417187950042E-16, 0.000000000000000000, 1.000000000000000000 ) ) ;
#11607 = LINE ( 'NONE', #11456, #8407 ) ;
#11608 = VERTEX_POINT ( 'NONE', #11399 ) ;
#11609 = CARTESIAN_POINT ( 'NONE',  ( -15.44029880530547416, -95.51755032243795540, -0.1252850382680660568 ) ) ;
#11610 = CARTESIAN_POINT ( 'NONE',  ( -15.61203582816999713, -108.0739631064533484, -6.614055049357310700 ) ) ;
#11611 = DIRECTION ( 'NONE',  ( 0.5975035461963189576, 0.8018662683283437342, 0.000000000000000000 ) ) ;
#11612 = DIRECTION ( 'NONE',  ( -1.000000000000000000, 0.000000000000000000, 0.000000000000000000 ) ) ;
#11613 = ORIENTED_EDGE ( 'NONE', *, *, #4422, .F. ) ;
#11614 = CARTESIAN_POINT ( 'NONE',  ( -7.568637282891814699, -45.56971093230124836, 46.82783525944628877 ) ) ;
#11615 = ORIENTED_EDGE ( 'NONE', *, *, #4497, .F. ) ;
#11616 = CARTESIAN_POINT ( 'NONE',  ( -7.495514965259227225, -43.99345095228513713, 19.34627428653194769 ) ) ;
#11617 = CARTESIAN_POINT ( 'NONE',  ( -15.49969986081100082, -110.0806363094795728, -1.108957527449961233 ) ) ;
#11618 = LINE ( 'NONE', #12783, #14228 ) ;
#11619 = CARTESIAN_POINT ( 'NONE',  ( -7.176549351029851032, -19.07651164606311056, 60.77823124794023357 ) ) ;
#11620 = CARTESIAN_POINT ( 'NONE',  ( -16.83285638980149201, -102.1523308006444353, -6.350246033081615948 ) ) ;
#11621 = CARTESIAN_POINT ( 'NONE',  ( -38.20335605883195029, -37.00737899243799234, 49.35084074737085302 ) ) ;
#11622 = DIRECTION ( 'NONE',  ( -0.4999999999999998890, 0.8660254037844387076, 0.000000000000000000 ) ) ;
#11623 = ORIENTED_EDGE ( 'NONE', *, *, #549, .F. ) ;
#11624 = CARTESIAN_POINT ( 'NONE',  ( -9.401538680480957311, -6.786242167561306715, 56.85231026484398598 ) ) ;
#11625 = ORIENTED_EDGE ( 'NONE', *, *, #13195, .T. ) ;
#11626 = CARTESIAN_POINT ( 'NONE',  ( -10.72806301968316411, -20.63252684047564500, 56.85231026484400019 ) ) ;
#11628 = ORIENTED_EDGE ( 'NONE', *, *, #7217, .T. ) ;
#11627 = CARTESIAN_POINT ( 'NONE',  ( -16.80342572160717651, -3.572236342509832241, 61.69496154213114636 ) ) ;
#11629 = EDGE_CURVE ( 'NONE', #12982, #8725, #7793, .T. ) ;
#11630 = ORIENTED_EDGE ( 'NONE', *, *, #2819, .T. ) ;
#11631 = ADVANCED_FACE ( 'NONE', ( #10251 ), #4289, .T. ) ;
#11632 = DIRECTION ( 'NONE',  ( -8.018662683283439195E-16, 5.975035461963190001E-16, 1.000000000000000000 ) ) ;
#11633 = ORIENTED_EDGE ( 'NONE', *, *, #6273, .F. ) ;
#11634 = CIRCLE ( 'NONE', #6245, 4.500000000000000000 ) ;
#11635 = CARTESIAN_POINT ( 'NONE',  ( -9.989347722329673829, -46.50737899243799944, -5.497689735156000346 ) ) ;
#11636 = CARTESIAN_POINT ( 'NONE',  ( -14.61203582817000068, -107.8163049764641812, -5.262754992868532433 ) ) ;
#11637 = CYLINDRICAL_SURFACE ( 'NONE', #5625, 8.000000000000000000 ) ;
#11638 = DIRECTION ( 'NONE',  ( 1.000000000000000000, 0.000000000000000000, 0.000000000000000000 ) ) ;
#11639 = CARTESIAN_POINT ( 'NONE',  ( 17.24950932937950299, -23.81275511923810839, 5.938204047008457387 ) ) ;
#11640 = VECTOR ( 'NONE', #2122, 1000.000000000000114 ) ;
#11641 = CARTESIAN_POINT ( 'NONE',  ( -16.58783302151896777, -10.98181643637917304, 56.75231026484397745 ) ) ;
#11642 = CARTESIAN_POINT ( 'NONE',  ( -28.78282149594069850, -32.00737899243799944, 59.28069236156870403 ) ) ;
#11643 = EDGE_LOOP ( 'NONE', ( #11142, #9645, #5090, #1261 ) ) ;
#11644 = CARTESIAN_POINT ( 'NONE',  ( -15.49969986081099371, -18.00737899243799944, -13.28793577849899776 ) ) ;
#11645 = ORIENTED_EDGE ( 'NONE', *, *, #6844, .F. ) ;
#11646 = DIRECTION ( 'NONE',  ( -0.6601155939154574881, 0.7511640317997414495, -9.781476007338062700E-16 ) ) ;
#11647 = VERTEX_POINT ( 'NONE', #1000 ) ;
#11648 = COLOUR_RGB ( '', 0.31764706, 0.68627451, 0.89019608) ;
#11649 = ORIENTED_EDGE ( 'NONE', *, *, #6558, .F. ) ;
#11650 = EDGE_CURVE ( 'NONE', #11072, #5306, #4442, .T. ) ;
#11651 = CARTESIAN_POINT ( 'NONE',  ( 6.329928126373893349, -37.10979894228395182, 50.00103417101053083 ) ) ;
#11652 = EDGE_LOOP ( 'NONE', ( #6052, #6961, #9752, #3735 ) ) ;
#11653 = DIRECTION ( 'NONE',  ( 0.000000000000000000, -1.000000000000000000, -1.224646799147350002E-16 ) ) ;
#11654 = PRESENTATION_STYLE_ASSIGNMENT (( #5687 ) ) ;
#11655 = DIRECTION ( 'NONE',  ( 0.5975035461963189576, 0.8018662683283437342, 0.000000000000000000 ) ) ;
#11656 = CARTESIAN_POINT ( 'NONE',  ( -23.49969986081099904, -44.50737899243799944, 19.50231026484399877 ) ) ;
#11658 = CARTESIAN_POINT ( 'NONE',  ( -33.49969986081099904, -51.00737899243799944, 19.50231026484398456 ) ) ;
#11657 = LINE ( 'NONE', #8134, #2772 ) ;
#11659 = VERTEX_POINT ( 'NONE', #12479 ) ;
#11660 = LINE ( 'NONE', #5018, #13160 ) ;
#11661 = CIRCLE ( 'NONE', #7981, 9.974999999999999645 ) ;
#11662 = DIRECTION ( 'NONE',  ( -8.018662683283438208E-16, 5.975035461963189015E-16, 1.000000000000000000 ) ) ;
#11663 = ORIENTED_EDGE ( 'NONE', *, *, #15072, .T. ) ;
#11664 = VERTEX_POINT ( 'NONE', #3297 ) ;
#11665 = FACE_OUTER_BOUND ( 'NONE', #9901, .T. ) ;
#11666 = EDGE_CURVE ( 'NONE', #13942, #7657, #5203, .T. ) ;
#11667 = VECTOR ( 'NONE', #9223, 1000.000000000000000 ) ;
#11668 = DIRECTION ( 'NONE',  ( 8.018662683283438208E-16, -5.975035461963189015E-16, -1.000000000000000000 ) ) ;
#11669 = ORIENTED_EDGE ( 'NONE', *, *, #3176, .T. ) ;
#11670 = DIRECTION ( 'NONE',  ( 0.000000000000000000, 0.1872998510044689147, 0.9823027872370635460 ) ) ;
#11671 = VERTEX_POINT ( 'NONE', #3141 ) ;
#11672 = EDGE_CURVE ( 'NONE', #3526, #10020, #8620, .T. ) ;
#11673 = DIRECTION ( 'NONE',  ( -0.9320450512859435044, 0.1973458207444490631, 0.3038859151196097730 ) ) ;
#11674 = AXIS2_PLACEMENT_3D ( 'NONE', #10595, #11817, #2340 ) ;
#11675 = CARTESIAN_POINT ( 'NONE',  ( -14.71582029074517095, -23.50178099748875837, 57.00081750421114890 ) ) ;
#11676 = VECTOR ( 'NONE', #693, 1000.000000000000000 ) ;
#11677 = EDGE_CURVE ( 'NONE', #1582, #2365, #1995, .T. ) ;
#11678 = LINE ( 'NONE', #10530, #158 ) ;
#11679 = CARTESIAN_POINT ( 'NONE',  ( -20.39403028972282428, -7.084672814149619136, 56.85231026484398598 ) ) ;
#11680 = VERTEX_POINT ( 'NONE', #12791 ) ;
#11681 = CARTESIAN_POINT ( 'NONE',  ( -6.507973901336479017, -12.27851192488648024, 57.00231026484399166 ) ) ;
#11682 = CARTESIAN_POINT ( 'NONE',  ( -20.44787060326519423, -4.846187890544671362, 56.85231026484398598 ) ) ;
#11683 = CARTESIAN_POINT ( 'NONE',  ( -15.49969986081099904, -32.00737899243799944, 24.21206422150099868 ) ) ;
#11684 = ADVANCED_FACE ( 'NONE', ( #13850 ), #6643, .F. ) ;
#11686 = EDGE_CURVE ( 'NONE', #8808, #13353, #11327, .T. ) ;
#11685 = CARTESIAN_POINT ( 'NONE',  ( -12.32172653804166096, -7.186294389320899256, 57.00231026484397745 ) ) ;
#11687 = ORIENTED_EDGE ( 'NONE', *, *, #9889, .T. ) ;
#11688 = DIRECTION ( 'NONE',  ( 0.9673062255102897744, -0.2536112499260168573, 9.271838545667874758E-16 ) ) ;
#11689 = ORIENTED_EDGE ( 'NONE', *, *, #10908, .F. ) ;
#11690 = DIRECTION ( 'NONE',  ( 0.5975035461963188466, 0.8018662683283437342, 0.000000000000000000 ) ) ;
#11691 = LINE ( 'NONE', #12782, #2407 ) ;
#11692 = CARTESIAN_POINT ( 'NONE',  ( -21.45979773411920277, -21.50599501901345434, 57.00231026484397745 ) ) ;
#11693 = LINE ( 'NONE', #4664, #4274 ) ;
#11694 = VECTOR ( 'NONE', #14483, 999.9999999999998863 ) ;
#11695 = LINE ( 'NONE', #1218, #11165 ) ;
#11696 = DIRECTION ( 'NONE',  ( 0.000000000000000000, 0.000000000000000000, 1.000000000000000000 ) ) ;
#11697 = LINE ( 'NONE', #12492, #7095 ) ;
#11698 = CARTESIAN_POINT ( 'NONE',  ( -35.37586185869766808, -38.10176464241880012, 51.30163939567694342 ) ) ;
#11699 = DIRECTION ( 'NONE',  ( 1.000000000000000000, 1.000000000000000078E-15, 0.000000000000000000 ) ) ;
#11700 = EDGE_LOOP ( 'NONE', ( #6445, #135, #1245, #11424 ) ) ;
#11701 = PLANE ( 'NONE',  #7362 ) ;
#11702 = UNCERTAINTY_MEASURE_WITH_UNIT (LENGTH_MEASURE( 1.000000000000000082E-05 ), #10339, 'distance_accuracy_value', 'NONE');
#11703 = EDGE_CURVE ( 'NONE', #3333, #7744, #2222, .T. ) ;
#11704 = VECTOR ( 'NONE', #7259, 1000.000000000000000 ) ;
#11705 = VERTEX_POINT ( 'NONE', #6868 ) ;
#11707 = ORIENTED_EDGE ( 'NONE', *, *, #5057, .F. ) ;
#11706 = CARTESIAN_POINT ( 'NONE',  ( -15.49969986081099904, -57.00737899243800655, 19.50231026484399877 ) ) ;
#11708 = VERTEX_POINT ( 'NONE', #1075 ) ;
#11709 = AXIS2_PLACEMENT_3D ( 'NONE', #2540, #10801, #14090 ) ;
#11710 = CARTESIAN_POINT ( 'NONE',  ( -16.99345872630171428, -15.51204466325908982, 51.00231026484399166 ) ) ;
#11711 = ORIENTED_EDGE ( 'NONE', *, *, #6343, .F. ) ;
#11712 = CARTESIAN_POINT ( 'NONE',  ( -28.78282149594069850, -31.14135358865360104, -10.85656391856669778 ) ) ;
#11713 = DIRECTION ( 'NONE',  ( 0.5975035461963188466, 0.8018662683283437342, 0.000000000000000000 ) ) ;
#11714 =( LENGTH_UNIT ( ) NAMED_UNIT ( * ) SI_UNIT ( .MILLI., .METRE. ) );
#11715 = LINE ( 'NONE', #13035, #5096 ) ;
#11716 = CIRCLE ( 'NONE', #245, 0.4500000000000011768 ) ;
#11717 = EDGE_CURVE ( 'NONE', #8623, #5152, #8862, .T. ) ;
#11718 = DIRECTION ( 'NONE',  ( 0.000000000000000000, 1.000000000000000000, 1.224646799147350002E-16 ) ) ;
#11719 = CARTESIAN_POINT ( 'NONE',  ( -14.41156670010287577, -16.03294154849727704, 56.75231026484399166 ) ) ;
#11720 = ORIENTED_EDGE ( 'NONE', *, *, #6485, .F. ) ;
#11721 = CARTESIAN_POINT ( 'NONE',  ( -23.14528701667493849, -16.10665716956490812, 57.00231026484397745 ) ) ;
#11722 = ORIENTED_EDGE ( 'NONE', *, *, #3080, .F. ) ;
#11723 = EDGE_LOOP ( 'NONE', ( #9160, #4064 ) ) ;
#11724 = ORIENTED_EDGE ( 'NONE', *, *, #5160, .F. ) ;
#11725 = CARTESIAN_POINT ( 'NONE',  ( 3.682457005310663334, -38.77348753606410270, 51.72516835908339772 ) ) ;
#11726 = EDGE_LOOP ( 'NONE', ( #1042, #5694, #14293, #14295 ) ) ;
#11727 = DIRECTION ( 'NONE',  ( 8.018662683283438208E-16, -5.975035461963189015E-16, -1.000000000000000000 ) ) ;
#11728 = DIRECTION ( 'NONE',  ( 1.000000000000000000, 1.000000000000000078E-15, 1.000000000000000078E-15 ) ) ;
#11729 = CARTESIAN_POINT ( 'NONE',  ( -12.56680741991290340, -91.35574364345187348, -10.00076552370670768 ) ) ;
#11730 = EDGE_CURVE ( 'NONE', #1022, #6280, #13037, .T. ) ;
#11731 = B_SPLINE_CURVE_WITH_KNOTS ( 'NONE', 3,
 ( #5635, #13977, #5932, #13828 ),
 .UNSPECIFIED., .F., .F.,
 ( 4, 4 ),
 ( 0.000000000000000000, 1.000000000000000000 ),
 .UNSPECIFIED. ) ;
#11732 = DIRECTION ( 'NONE',  ( 0.000000000000000000, 0.000000000000000000, 1.000000000000000000 ) ) ;
#11734 = CARTESIAN_POINT ( 'NONE',  ( -38.39232659951203175, 4.291769771411864554, 26.45343327543596956 ) ) ;
#11733 = CYLINDRICAL_SURFACE ( 'NONE', #6423, 0.4000000000000002998 ) ;
#11735 = VERTEX_POINT ( 'NONE', #7096 ) ;
#11736 = DIRECTION ( 'NONE',  ( 0.000000000000000000, -1.000000000000000000, -1.224646799147350002E-16 ) ) ;
#11737 = CARTESIAN_POINT ( 'NONE',  ( -19.54308590270338541, -15.50439178786203342, -13.06948577250756927 ) ) ;
#11738 = ORIENTED_EDGE ( 'NONE', *, *, #5233, .F. ) ;
#11739 = VERTEX_POINT ( 'NONE', #315 ) ;
#11740 = CARTESIAN_POINT ( 'NONE',  ( 21.87349421687013518, -28.05917899276372296, 27.29443387538804444 ) ) ;
#11741 = CARTESIAN_POINT ( 'NONE',  ( -9.539601987502637215, -5.508762965862999295, 54.00231026484399166 ) ) ;
#11742 = ORIENTED_EDGE ( 'NONE', *, *, #7449, .T. ) ;
#11743 =( BOUNDED_CURVE ( )  B_SPLINE_CURVE ( 3, ( #13479, #5433, #12401, #12254 ),
 .UNSPECIFIED., .F., .F. ) 
 B_SPLINE_CURVE_WITH_KNOTS ( ( 4, 4 ),
 ( 3.141592653589793560, 4.712388980384691450 ),
 .UNSPECIFIED. ) 
 CURVE ( )  GEOMETRIC_REPRESENTATION_ITEM ( )  RATIONAL_B_SPLINE_CURVE ( ( 1.000000000000000000, 0.8047378541243646044, 0.8047378541243646044, 1.000000000000000000 ) ) 
 REPRESENTATION_ITEM ( '' )  );
#11744 = PRESENTATION_STYLE_ASSIGNMENT (( #7144 ) ) ;
#11745 = ORIENTED_EDGE ( 'NONE', *, *, #9923, .T. ) ;
#11746 = DIRECTION ( 'NONE',  ( 0.000000000000000000, -0.6540809579092761172, -0.7564245504347962834 ) ) ;
#11747 = AXIS2_PLACEMENT_3D ( 'NONE', #3848, #6126, #13898 ) ;
#11748 = ADVANCED_FACE ( 'NONE', ( #10 ), #4905, .T. ) ;
#11749 = DIRECTION ( 'NONE',  ( -8.018662683283438208E-16, 5.975035461963189015E-16, 1.000000000000000000 ) ) ;
#11750 = CARTESIAN_POINT ( 'NONE',  ( -15.49969986081099904, 4.873818854044997373, 47.21206422150099513 ) ) ;
#11751 = EDGE_CURVE ( 'NONE', #5899, #9493, #9364, .T. ) ;
#11752 = ORIENTED_EDGE ( 'NONE', *, *, #2059, .T. ) ;
#11753 = DIRECTION ( 'NONE',  ( -8.673617379884027583E-16, 1.000000000000000000, 0.000000000000000000 ) ) ;
#11754 = DIRECTION ( 'NONE',  ( 4.999999999999998416E-16, -0.4999999999999998890, 0.8660254037844387076 ) ) ;
#11755 = ORIENTED_EDGE ( 'NONE', *, *, #14674, .F. ) ;
#11756 = CARTESIAN_POINT ( 'NONE',  ( -15.10625462230756000, -3.540141368888815254, 54.00231026484397745 ) ) ;
#11757 = VERTEX_POINT ( 'NONE', #9408 ) ;
#11758 = DIRECTION ( 'NONE',  ( 0.5975035461963189576, 0.8018662683283437342, 0.000000000000000000 ) ) ;
#11759 = EDGE_LOOP ( 'NONE', ( #7370, #703, #2944, #238 ) ) ;
#11760 = VECTOR ( 'NONE', #14078, 1000.000000000000000 ) ;
#11761 = LINE ( 'NONE', #1285, #2503 ) ;
#11762 = CARTESIAN_POINT ( 'NONE',  ( -8.744338604334316756, -15.61126689213601360, 56.85231026484400019 ) ) ;
#11763 = CARTESIAN_POINT ( 'NONE',  ( -15.49969986081099904, -107.1622034095870077, -6.087689735155999315 ) ) ;
#11764 = DIRECTION ( 'NONE',  ( 1.000000000000000000, 1.201369187114119994E-15, 9.616040805000176517E-16 ) ) ;
#11765 = CARTESIAN_POINT ( 'NONE',  ( -7.949896068685645467, -47.15850730160504867, 46.92147361607200651 ) ) ;
#11766 = ADVANCED_FACE ( 'NONE', ( #6101 ), #14233, .T. ) ;
#11767 = DIRECTION ( 'NONE',  ( -8.018662683283438208E-16, 5.975035461963189015E-16, 1.000000000000000000 ) ) ;
#11768 = AXIS2_PLACEMENT_3D ( 'NONE', #7894, #8902, #13580 ) ;
#11769 = EDGE_CURVE ( 'NONE', #6348, #8564, #2525, .T. ) ;
#11770 = AXIS2_PLACEMENT_3D ( 'NONE', #7764, #466, #5124 ) ;
#11771 = VECTOR ( 'NONE', #15062, 1000.000000000000000 ) ;
#11772 = FACE_OUTER_BOUND ( 'NONE', #1597, .T. ) ;
#11773 = EDGE_CURVE ( 'NONE', #6233, #6946, #7331, .T. ) ;
#11774 = ORIENTED_EDGE ( 'NONE', *, *, #4683, .F. ) ;
#11775 = CARTESIAN_POINT ( 'NONE',  ( -23.49969986081099904, -19.50737899243800300, 48.00231026484399877 ) ) ;
#11776 = LINE ( 'NONE', #6940, #4855 ) ;
#11777 = FACE_OUTER_BOUND ( 'NONE', #8860, .T. ) ;
#11778 = ORIENTED_EDGE ( 'NONE', *, *, #474, .T. ) ;
#11779 = DIRECTION ( 'NONE',  ( -1.000000000000000000, -1.000000000000000078E-15, 0.000000000000000000 ) ) ;
#11780 = EDGE_LOOP ( 'NONE', ( #13634, #450, #6947, #5898 ) ) ;
#11782 = EDGE_LOOP ( 'NONE', ( #6684, #12374, #4671, #6141 ) ) ;
#11781 = DIRECTION ( 'NONE',  ( 0.000000000000000000, 0.000000000000000000, 1.000000000000000000 ) ) ;
#11783 = ADVANCED_FACE ( 'NONE', ( #2378 ), #7177, .T. ) ;
#11784 = ORIENTED_EDGE ( 'NONE', *, *, #4879, .T. ) ;
#11785 = AXIS2_PLACEMENT_3D ( 'NONE', #6913, #12677, #11444 ) ;
#11786 = DIRECTION ( 'NONE',  ( 0.000000000000000000, 0.1872998510044689147, 0.9823027872370635460 ) ) ;
#11787 = ORIENTED_EDGE ( 'NONE', *, *, #2519, .F. ) ;
#11788 = VECTOR ( 'NONE', #8565, 1000.000000000000000 ) ;
#11789 = CIRCLE ( 'NONE', #556, 0.2000000000000012046 ) ;
#11790 = DIRECTION ( 'NONE',  ( -8.018662683283438208E-16, 5.975035461963189015E-16, 1.000000000000000000 ) ) ;
#11791 = DIRECTION ( 'NONE',  ( -8.018662683283438208E-16, 5.975035461963189015E-16, 1.000000000000000000 ) ) ;
#11792 = CARTESIAN_POINT ( 'NONE',  ( -20.60611791317904107, -19.76323582219775687, 57.00231026484397745 ) ) ;
#11793 = DIRECTION ( 'NONE',  ( 0.000000000000000000, 0.000000000000000000, 1.000000000000000000 ) ) ;
#11794 = ADVANCED_FACE ( 'NONE', ( #11777 ), #9484, .F. ) ;
#11795 = CARTESIAN_POINT ( 'NONE',  ( 18.17286069890486644, -24.91224770180716419, 7.706609472668462857 ) ) ;
#11796 = LINE ( 'NONE', #14675, #3288 ) ;
#11797 = AXIS2_PLACEMENT_3D ( 'NONE', #9655, #14095, #13038 ) ;
#11798 = DIRECTION ( 'NONE',  ( 0.000000000000000000, 0.000000000000000000, 1.000000000000000000 ) ) ;
#11799 = CARTESIAN_POINT ( 'NONE',  ( 4.595282735339393909, -37.93213861349479288, -12.15966626606534717 ) ) ;
#11800 = ORIENTED_EDGE ( 'NONE', *, *, #4912, .F. ) ;
#11801 = DIRECTION ( 'NONE',  ( 8.018662683283438208E-16, -5.975035461963189015E-16, -1.000000000000000000 ) ) ;
#11802 = ORIENTED_EDGE ( 'NONE', *, *, #13237, .F. ) ;
#11803 = VERTEX_POINT ( 'NONE', #13169 ) ;
#11804 = DIRECTION ( 'NONE',  ( 0.5975035461963188466, 0.8018662683283437342, 0.000000000000000000 ) ) ;
#11805 = ORIENTED_EDGE ( 'NONE', *, *, #4626, .F. ) ;
#11807 = EDGE_CURVE ( 'NONE', #609, #970, #6025, .T. ) ;
#11806 = CARTESIAN_POINT ( 'NONE',  ( 22.00030013918900096, -27.00737899243800300, 24.21206422150099868 ) ) ;
#11808 = VECTOR ( 'NONE', #7246, 1000.000000000000000 ) ;
#11809 = PRESENTATION_STYLE_ASSIGNMENT (( #3852 ) ) ;
#11810 = DIRECTION ( 'NONE',  ( -8.018662683283438208E-16, 5.975035461963189015E-16, 1.000000000000000000 ) ) ;
#11811 = VECTOR ( 'NONE', #3023, 1000.000000000000114 ) ;
#11812 = VECTOR ( 'NONE', #4410, 1000.000000000000000 ) ;
#11813 = CARTESIAN_POINT ( 'NONE',  ( -15.24029490235350259, -21.57855976525750563, 56.85231026484400019 ) ) ;
#11815 = CYLINDRICAL_SURFACE ( 'NONE', #11450, 2.999999999999999112 ) ;
#11814 = CARTESIAN_POINT ( 'NONE',  ( -7.504576870302558156, -44.41851609332119466, 20.88336806361667897 ) ) ;
#11816 = ORIENTED_EDGE ( 'NONE', *, *, #2763, .T. ) ;
#11817 = DIRECTION ( 'NONE',  ( 8.018662683283438208E-16, -5.975035461963189015E-16, -1.000000000000000000 ) ) ;
#11818 = CARTESIAN_POINT ( 'NONE',  ( -23.49969986081099904, -19.50737899243800300, 60.84879442494580104 ) ) ;
#11819 = EDGE_LOOP ( 'NONE', ( #11242, #6664, #10831, #9663 ) ) ;
#11820 = EDGE_LOOP ( 'NONE', ( #14194, #9662 ) ) ;
#11821 = DIRECTION ( 'NONE',  ( 8.018662683283438208E-16, -5.975035461963189015E-16, -1.000000000000000000 ) ) ;
#11822 = AXIS2_PLACEMENT_3D ( 'NONE', #9215, #973, #9142 ) ;
#11823 = CARTESIAN_POINT ( 'NONE',  ( -15.49969986081099904, 20.99262100756199700, 47.21206422150099513 ) ) ;
#11824 = ORIENTED_EDGE ( 'NONE', *, *, #5335, .F. ) ;
#11825 = CARTESIAN_POINT ( 'NONE',  ( -24.05607732349520234, -14.07716379046991584, 56.85231026484398598 ) ) ;
#11826 = EDGE_CURVE ( 'NONE', #10111, #6762, #1299, .T. ) ;
#11827 = EDGE_CURVE ( 'NONE', #5287, #5522, #1876, .T. ) ;
#11828 = VECTOR ( 'NONE', #5786, 1000.000000000000114 ) ;
#11829 = LINE ( 'NONE', #11905, #9512 ) ;
#11830 = CIRCLE ( 'NONE', #5467, 0.4500000000000011768 ) ;
#11831 = DIRECTION ( 'NONE',  ( -0.9966498018049937402, 0.08178736187251965661, -8.480480961564258050E-16 ) ) ;
#11832 = CARTESIAN_POINT ( 'NONE',  ( -22.00391959472895209, -7.178368354675633611, 56.85231026484398598 ) ) ;
#11833 = DIRECTION ( 'NONE',  ( -0.000000000000000000, 0.000000000000000000, -1.000000000000000000 ) ) ;
#11834 = ORIENTED_EDGE ( 'NONE', *, *, #10067, .T. ) ;
#11835 = CARTESIAN_POINT ( 'NONE',  ( -11.55178736972959896, -19.37894070656198764, 56.85231026484400019 ) ) ;
#11836 =( BOUNDED_CURVE ( )  B_SPLINE_CURVE ( 3, ( #8777, #9925, #10232, #12307 ),
 .UNSPECIFIED., .F., .T. ) 
 B_SPLINE_CURVE_WITH_KNOTS ( ( 4, 4 ),
 ( 5.074465175390796112, 5.274925224928544765 ),
 .UNSPECIFIED. ) 
 CURVE ( )  GEOMETRIC_REPRESENTATION_ITEM ( )  RATIONAL_B_SPLINE_CURVE ( ( 1.000000000000000000, 0.9966541165307394312, 0.9966541165307394312, 1.000000000000000000 ) ) 
 REPRESENTATION_ITEM ( '' )  );
#11837 = CARTESIAN_POINT ( 'NONE',  ( -15.49969986081099904, -13.50737899243800122, 54.00231026484400587 ) ) ;
#11838 = ORIENTED_EDGE ( 'NONE', *, *, #14864, .T. ) ;
#11839 = LINE ( 'NONE', #11756, #13667 ) ;
#11840 = ORIENTED_EDGE ( 'NONE', *, *, #11063, .F. ) ;
#11841 = CARTESIAN_POINT ( 'NONE',  ( 22.00030013918900096, -27.00737899243800300, 7.712064221501001349 ) ) ;
#11842 = ORIENTED_EDGE ( 'NONE', *, *, #1201, .T. ) ;
#11843 = VECTOR ( 'NONE', #14990, 1000.000000000000000 ) ;
#11844 = ADVANCED_FACE ( 'NONE', ( #13091 ), #1454, .T. ) ;
#11845 = FACE_OUTER_BOUND ( 'NONE', #12274, .T. ) ;
#11846 = PLANE ( 'NONE',  #9970 ) ;
#11847 = LINE ( 'NONE', #153, #4041 ) ;
#11848 = LINE ( 'NONE', #13312, #9836 ) ;
#11849 = DIRECTION ( 'NONE',  ( -0.6519834208811554621, -0.7582332219680868457, -6.975647374412761332E-17 ) ) ;
#11850 = DIRECTION ( 'NONE',  ( 0.000000000000000000, 1.000000000000000000, 1.224646799147350002E-16 ) ) ;
#11851 = AXIS2_PLACEMENT_3D ( 'NONE', #2834, #2912, #13180 ) ;
#11852 = CARTESIAN_POINT ( 'NONE',  ( 14.77505403666262040, -27.91489101255499250, 2.083060336410837987 ) ) ;
#11853 = VERTEX_POINT ( 'NONE', #3676 ) ;
#11854 = FACE_OUTER_BOUND ( 'NONE', #648, .T. ) ;
#11855 = CARTESIAN_POINT ( 'NONE',  ( -37.02289807341878713, -37.22897031456928119, 50.21085258507981308 ) ) ;
#11856 = DIRECTION ( 'NONE',  ( 0.9983330752162417054, 0.05771543059946734194, 7.660444431189781397E-16 ) ) ;
#11857 = VERTEX_POINT ( 'NONE', #12013 ) ;
#11858 = CARTESIAN_POINT ( 'NONE',  ( -15.49969986081092088, -13.50737899243822504, 57.00231026484397745 ) ) ;
#11859 = ORIENTED_EDGE ( 'NONE', *, *, #3283, .F. ) ;
#11861 = ORIENTED_EDGE ( 'NONE', *, *, #8170, .F. ) ;
#11860 = DIRECTION ( 'NONE',  ( 0.000000000000000000, 1.850371707708594316E-16, -1.000000000000000000 ) ) ;
#11862 = ORIENTED_EDGE ( 'NONE', *, *, #8152, .F. ) ;
#11863 = ADVANCED_FACE ( 'NONE', ( #5806 ), #10482, .T. ) ;
#11864 = PLANE ( 'NONE',  #11911 ) ;
#11865 = ORIENTED_EDGE ( 'NONE', *, *, #372, .F. ) ;
#11866 = EDGE_CURVE ( 'NONE', #4633, #12536, #12863, .T. ) ;
#11867 = CARTESIAN_POINT ( 'NONE',  ( -15.49969986081099904, 10.68321993080349763, 24.21206422150099868 ) ) ;
#11868 = DIRECTION ( 'NONE',  ( 0.000000000000000000, -1.000000000000000000, -1.224646799147350002E-16 ) ) ;
#11869 = DIRECTION ( 'NONE',  ( 9.869715661189562567E-16, -0.9869715661189463196, -0.1608947720490454258 ) ) ;
#11870 = EDGE_CURVE ( 'NONE', #8946, #3470, #2899, .T. ) ;
#11871 = DIRECTION ( 'NONE',  ( 0.1165201156931293391, 0.9931883319083343320, -4.999999999999998416E-16 ) ) ;
#11872 = LINE ( 'NONE', #254, #13997 ) ;
#11873 = VERTEX_POINT ( 'NONE', #10096 ) ;
#11874 = CARTESIAN_POINT ( 'NONE',  ( 2.500300139189003623, -41.64411882298843892, -13.39525803434795570 ) ) ;
#11875 = EDGE_LOOP ( 'NONE', ( #2240, #7698, #912, #12076 ) ) ;
#11876 = VECTOR ( 'NONE', #6097, 1000.000000000000000 ) ;
#11877 = LINE ( 'NONE', #8431, #2853 ) ;
#11878 = VERTEX_POINT ( 'NONE', #5289 ) ;
#11879 = ORIENTED_EDGE ( 'NONE', *, *, #12415, .T. ) ;
#11880 = EDGE_CURVE ( 'NONE', #14409, #14119, #6496, .T. ) ;
#11881 = LINE ( 'NONE', #6051, #3459 ) ;
#11882 = EDGE_CURVE ( 'NONE', #12018, #10291, #9883, .T. ) ;
#11883 = ORIENTED_EDGE ( 'NONE', *, *, #3273, .F. ) ;
#11884 = CARTESIAN_POINT ( 'NONE',  ( -6.726903101582546007, -11.18374239837452500, 57.00231026484399166 ) ) ;
#11885 = CARTESIAN_POINT ( 'NONE',  ( -9.539601987502633662, -5.508762965863001071, 51.00231026484399166 ) ) ;
#11886 = CARTESIAN_POINT ( 'NONE',  ( -28.78282149594069850, -32.00737899243799944, 24.21206422150099868 ) ) ;
#11887 = LINE ( 'NONE', #10589, #10222 ) ;
#11888 = VECTOR ( 'NONE', #12638, 1000.000000000000114 ) ;
#11889 = DIRECTION ( 'NONE',  ( 0.000000000000000000, -2.185478394931410082E-16, 1.000000000000000000 ) ) ;
#11891 = CARTESIAN_POINT ( 'NONE',  ( -22.56290636796585503, -13.91571566392944526, 56.85231026484398598 ) ) ;
#11890 = CARTESIAN_POINT ( 'NONE',  ( -7.649802761028805520, -48.47628348355120664, -3.956830880212969248 ) ) ;
#11892 = ORIENTED_EDGE ( 'NONE', *, *, #4070, .F. ) ;
#11893 = CARTESIAN_POINT ( 'NONE',  ( -13.09722856071139496, -21.21670818843173478, 56.85231026484400019 ) ) ;
#11894 = LINE ( 'NONE', #14272, #9854 ) ;
#11895 = ORIENTED_EDGE ( 'NONE', *, *, #12561, .F. ) ;
#11896 = VERTEX_POINT ( 'NONE', #4147 ) ;
#11897 = CARTESIAN_POINT ( 'NONE',  ( 21.96544832021356441, -29.82936669528688967, 25.83808190157214568 ) ) ;
#11898 = DIRECTION ( 'NONE',  ( 1.000000000000000000, -1.291538348938060198E-32, 1.054621095516909827E-16 ) ) ;
#11899 = CIRCLE ( 'NONE', #9691, 23.00000000000000000 ) ;
#11900 = EDGE_CURVE ( 'NONE', #5530, #3694, #3183, .T. ) ;
#11901 = ORIENTED_EDGE ( 'NONE', *, *, #5778, .F. ) ;
#11902 = CARTESIAN_POINT ( 'NONE',  ( -10.83829729829802169, -38.00046876589347278, -17.70749226439889412 ) ) ;
#11903 = B_SPLINE_CURVE_WITH_KNOTS ( 'NONE', 3,
 ( #12754, #7915, #4487, #10370, #14892, #8991, #11294, #4415, #823, #1113, #5626, #3336, #9067, #10293, #13743, #5703, #13673, #7987, #14964, #5772, #15037, #3486, #4561 ),
 .UNSPECIFIED., .F., .F.,
 ( 4, 2, 1, 2, 2, 2, 2, 2, 2, 2, 2, 4 ),
 ( 0.01260730609128223219, 0.01339570877218145863, 0.01418411145308068333, 0.01497251413397990977, 0.01576091681487913621, 0.01733772217667757867, 0.01891452753847602461, 0.02049133290027446708, 0.02127973558117368311, 0.02206813826207289914, 0.02364494362387132426, 0.02522174898566975285 ),
 .UNSPECIFIED. ) ;
#11904 = VECTOR ( 'NONE', #2306, 1000.000000000000000 ) ;
#11905 = CARTESIAN_POINT ( 'NONE',  ( -17.61203582817000068, -107.3963282233425645, -7.315568219202336131 ) ) ;
#11906 = CARTESIAN_POINT ( 'NONE',  ( 1.760741030006599317, 10.68321993080349763, 16.26994987741148790 ) ) ;
#11907 = VECTOR ( 'NONE', #2583, 1000.000000000000000 ) ;
#11908 = EDGE_CURVE ( 'NONE', #6605, #6877, #14502, .T. ) ;
#11909 = CARTESIAN_POINT ( 'NONE',  ( -15.53608329785963527, -13.54167542823733328, 56.85231026484398598 ) ) ;
#11910 = CARTESIAN_POINT ( 'NONE',  ( -15.49969986081099904, 64.39262100756199914, 29.46206422150100934 ) ) ;
#11911 = AXIS2_PLACEMENT_3D ( 'NONE', #10641, #1082, #9415 ) ;
#11912 = EDGE_LOOP ( 'NONE', ( #7583, #7316, #1923, #11217 ) ) ;
#11913 = FACE_OUTER_BOUND ( 'NONE', #6309, .T. ) ;
#11914 = DIRECTION ( 'NONE',  ( 1.000000000000000000, 1.000000000000000078E-15, 0.000000000000000000 ) ) ;
#11915 = VERTEX_POINT ( 'NONE', #12258 ) ;
#11916 = CARTESIAN_POINT ( 'NONE',  ( -7.510805280342158774, -44.08454818175437850, 18.85714484343347408 ) ) ;
#11917 = FILL_AREA_STYLE ('',( #2155 ) ) ;
#11918 = ORIENTED_EDGE ( 'NONE', *, *, #8188, .T. ) ;
#11919 = DIRECTION ( 'NONE',  ( 0.5975035461963189576, 0.8018662683283437342, 0.000000000000000000 ) ) ;
#11920 = ORIENTED_EDGE ( 'NONE', *, *, #12500, .F. ) ;
#11921 = CARTESIAN_POINT ( 'NONE',  ( -15.49969986081086226, -13.50737899243826767, -13.99768973515600301 ) ) ;
#11922 = CYLINDRICAL_SURFACE ( 'NONE', #790, 8.000000000000000000 ) ;
#11923 = DIRECTION ( 'NONE',  ( 0.000000000000000000, -1.000000000000000000, -1.224646799147350002E-16 ) ) ;
#11924 = VECTOR ( 'NONE', #11006, 1000.000000000000000 ) ;
#11925 = AXIS2_PLACEMENT_3D ( 'NONE', #13738, #8984, #10288 ) ;
#11926 = VECTOR ( 'NONE', #75, 1000.000000000000000 ) ;
#11927 = VECTOR ( 'NONE', #3021, 1000.000000000000000 ) ;
#11928 = CARTESIAN_POINT ( 'NONE',  ( -22.64031343690345111, -17.27870339600297811, 56.85231026484398598 ) ) ;
#11929 = LINE ( 'NONE', #2447, #7719 ) ;
#11930 =( BOUNDED_CURVE ( )  B_SPLINE_CURVE ( 3, ( #2589, #7001, #9396, #14063 ),
 .UNSPECIFIED., .F., .T. ) 
 B_SPLINE_CURVE_WITH_KNOTS ( ( 4, 4 ),
 ( 1.570796326794896114, 3.141592653589792672 ),
 .UNSPECIFIED. ) 
 CURVE ( )  GEOMETRIC_REPRESENTATION_ITEM ( )  RATIONAL_B_SPLINE_CURVE ( ( 1.000000000000000000, 0.8047378541243649375, 0.8047378541243649375, 1.000000000000000000 ) ) 
 REPRESENTATION_ITEM ( '' )  );
#11931 = EDGE_CURVE ( 'NONE', #3714, #11739, #13411, .T. ) ;
#11932 = LINE ( 'NONE', #2673, #3078 ) ;
#11933 = VERTEX_POINT ( 'NONE', #8803 ) ;
#11934 = DIRECTION ( 'NONE',  ( 0.000000000000000000, 0.000000000000000000, -1.000000000000000000 ) ) ;
#11935 = CARTESIAN_POINT ( 'NONE',  ( -33.49969986081099904, -42.00737899243800655, 52.39987856403599409 ) ) ;
#11936 = CARTESIAN_POINT ( 'NONE',  ( -24.05607732349520234, -14.07716379046991584, 57.00231026484397745 ) ) ;
#11937 = AXIS2_PLACEMENT_3D ( 'NONE', #12747, #8910, #4254 ) ;
#11938 = ORIENTED_EDGE ( 'NONE', *, *, #10569, .T. ) ;
#11939 = CARTESIAN_POINT ( 'NONE',  ( -7.501944906337848273, -44.50613385756380325, -4.001965388595783324 ) ) ;
#11940 = VERTEX_POINT ( 'NONE', #2995 ) ;
#11942 = VERTEX_POINT ( 'NONE', #14697 ) ;
#11941 = FACE_OUTER_BOUND ( 'NONE', #13524, .T. ) ;
#11943 = ORIENTED_EDGE ( 'NONE', *, *, #7637, .F. ) ;
#11944 = CARTESIAN_POINT ( 'NONE',  ( -22.86200450971638531, -18.81376385001357932, 56.85231026484398598 ) ) ;
#11945 = ORIENTED_EDGE ( 'NONE', *, *, #13313, .T. ) ;
#11946 = VECTOR ( 'NONE', #13492, 1000.000000000000114 ) ;
#11947 = LINE ( 'NONE', #12873, #1948 ) ;
#11948 = CARTESIAN_POINT ( 'NONE',  ( 0.8003001391889992266, 20.99262100756200056, 16.16206422150100153 ) ) ;
#11949 = DIRECTION ( 'NONE',  ( -8.018662683283439195E-16, 5.975035461963190001E-16, 1.000000000000000000 ) ) ;
#11950 = CARTESIAN_POINT ( 'NONE',  ( 0.000000000000000000, 0.000000000000000000, 0.000000000000000000 ) ) ;
#11951 = CARTESIAN_POINT ( 'NONE',  ( -19.97050308595844825, -12.91592837963194462, -13.02052021517568647 ) ) ;
#11952 = EDGE_CURVE ( 'NONE', #6007, #11221, #13630, .T. ) ;
#11953 = AXIS2_PLACEMENT_3D ( 'NONE', #6087, #11997, #1281 ) ;
#11954 = PRODUCT_DEFINITION_FORMATION_WITH_SPECIFIED_SOURCE ( 'ANY', '', #264, .NOT_KNOWN. ) ;
#11955 = CARTESIAN_POINT ( 'NONE',  ( -15.04562126104788966, -5.444807279564146896, 56.85231026484398598 ) ) ;
#11956 = EDGE_CURVE ( 'NONE', #2788, #2864, #7581, .T. ) ;
#11957 = CARTESIAN_POINT ( 'NONE',  ( 4.194495296137883855, -38.25609885807656951, -12.40989724287477891 ) ) ;
#11958 = ORIENTED_EDGE ( 'NONE', *, *, #3088, .T. ) ;
#11959 = CARTESIAN_POINT ( 'NONE',  ( 21.85920135429434907, -27.00737899243800300, 20.96206422150100224 ) ) ;
#11960 = VERTEX_POINT ( 'NONE', #7722 ) ;
#11961 = ORIENTED_EDGE ( 'NONE', *, *, #10207, .F. ) ;
#11962 = CARTESIAN_POINT ( 'NONE',  ( 3.853695978508554720, -38.58518656693815529, 51.62240523568905104 ) ) ;
#11963 = ORIENTED_EDGE ( 'NONE', *, *, #13475, .F. ) ;
#11964 = CARTESIAN_POINT ( 'NONE',  ( -25.46211945451987191, -14.00819915864900800, 56.85231026484398598 ) ) ;
#11965 = DIRECTION ( 'NONE',  ( -8.018662683283438208E-16, 5.975035461963189015E-16, 1.000000000000000000 ) ) ;
#11966 = AXIS2_PLACEMENT_3D ( 'NONE', #1628, #14557, #5079 ) ;
#11967 = EDGE_CURVE ( 'NONE', #6204, #8466, #628, .T. ) ;
#11968 = AXIS2_PLACEMENT_3D ( 'NONE', #6845, #9301, #5779 ) ;
#11969 = DIRECTION ( 'NONE',  ( -0.9931883319083343320, 0.1165201156931293391, -8.660254037844387408E-16 ) ) ;
#11970 = DIRECTION ( 'NONE',  ( -0.7582332219680868457, 0.6519834208811555731, -9.975640502598242007E-16 ) ) ;
#11971 = ADVANCED_FACE ( 'NONE', ( #7950 ), #14924, .F. ) ;
#11972 = EDGE_CURVE ( 'NONE', #3521, #1308, #6721, .T. ) ;
#11973 = CARTESIAN_POINT ( 'NONE',  ( -3.508527451664998686, -47.37340439622244048, -3.997689735156000790 ) ) ;
#11974 = CARTESIAN_POINT ( 'NONE',  ( -11.16775676328319200, -22.49263881059494707, 57.00231026484399166 ) ) ;
#11975 = EDGE_CURVE ( 'NONE', #7684, #2792, #8026, .T. ) ;
#11976 = ORIENTED_EDGE ( 'NONE', *, *, #2230, .F. ) ;
#11977 = CARTESIAN_POINT ( 'NONE',  ( -15.14850084941412511, -4.438867027711355107, 57.00231026484397745 ) ) ;
#11978 = FACE_OUTER_BOUND ( 'NONE', #5919, .T. ) ;
#11979 = ORIENTED_EDGE ( 'NONE', *, *, #866, .T. ) ;
#11980 = ORIENTED_EDGE ( 'NONE', *, *, #13468, .F. ) ;
#11981 = FACE_OUTER_BOUND ( 'NONE', #8543, .T. ) ;
#11982 = ORIENTED_EDGE ( 'NONE', *, *, #177, .T. ) ;
#11983 = FACE_OUTER_BOUND ( 'NONE', #10560, .T. ) ;
#11984 = EDGE_CURVE ( 'NONE', #8987, #3406, #11481, .T. ) ;
#11985 = AXIS2_PLACEMENT_3D ( 'NONE', #10587, #7127, #14263 ) ;
#11986 = FACE_OUTER_BOUND ( 'NONE', #11571, .T. ) ;
#11987 = CARTESIAN_POINT ( 'NONE',  ( -9.097666755470994460, -21.18944696257707250, 56.45155857467202054 ) ) ;
#11988 = UNCERTAINTY_MEASURE_WITH_UNIT (LENGTH_MEASURE( 1.000000000000000082E-05 ), #14278, 'distance_accuracy_value', 'NONE');
#11989 = ADVANCED_FACE ( 'NONE', ( #2079 ), #6412, .T. ) ;
#11990 = CARTESIAN_POINT ( 'NONE',  ( -20.36203582816999713, -107.3963282233425787, -7.315568219202339684 ) ) ;
#11991 = CARTESIAN_POINT ( 'NONE',  ( -19.41680297924232690, -22.68108752059492517, 57.00231026484399166 ) ) ;
#11993 = VERTEX_POINT ( 'NONE', #856 ) ;
#11992 = CIRCLE ( 'NONE', #9071, 5.000000000000000000 ) ;
#11994 = DIRECTION ( 'NONE',  ( 1.000000000000000000, 0.000000000000000000, 0.000000000000000000 ) ) ;
#11995 = FACE_OUTER_BOUND ( 'NONE', #1556, .T. ) ;
#11996 = ORIENTED_EDGE ( 'NONE', *, *, #14204, .T. ) ;
#11997 = DIRECTION ( 'NONE',  ( 0.000000000000000000, 1.000000000000000000, 1.224646799147350002E-16 ) ) ;
#11998 =( NAMED_UNIT ( * ) SI_UNIT ( $, .STERADIAN. ) SOLID_ANGLE_UNIT ( ) );
#11999 = ORIENTED_EDGE ( 'NONE', *, *, #9333, .T. ) ;
#12000 = DIRECTION ( 'NONE',  ( -8.018662683283438208E-16, 5.975035461963189015E-16, 1.000000000000000000 ) ) ;
#12001 = ORIENTED_EDGE ( 'NONE', *, *, #3812, .T. ) ;
#12002 = CARTESIAN_POINT ( 'NONE',  ( -9.884208147447518300, -5.263176313152190922, 56.85231026484398598 ) ) ;
#12003 = CARTESIAN_POINT ( 'NONE',  ( -6.309378268457435546, -9.629413800598410234, 56.85231026484400019 ) ) ;
#12004 = PRODUCT_DEFINITION ( 'UNKNOWN', '', #12940, #1302 ) ;
#12005 = ADVANCED_FACE ( 'NONE', ( #1148, #1079 ), #12639, .T. ) ;
#12006 = DIRECTION ( 'NONE',  ( 0.000000000000000000, 0.000000000000000000, 1.000000000000000000 ) ) ;
#12007 = CARTESIAN_POINT ( 'NONE',  ( -7.804240102366953202, -47.71020347972454090, 17.31052141267318234 ) ) ;
#12008 = CARTESIAN_POINT ( 'NONE',  ( 18.52099659588564862, -27.46909528396324518, 8.437240866514711612 ) ) ;
#12009 = VERTEX_POINT ( 'NONE', #11404 ) ;
#12010 = CARTESIAN_POINT ( 'NONE',  ( -15.49969986081099371, -52.50737899243799944, -17.99768973515599768 ) ) ;
#12011 = DIRECTION ( 'NONE',  ( 0.000000000000000000, 0.000000000000000000, -1.000000000000000000 ) ) ;
#12012 = VECTOR ( 'NONE', #9664, 1000.000000000000000 ) ;
#12013 = CARTESIAN_POINT ( 'NONE',  ( -23.40321606353253614, -15.16438883951732741, 56.85231026484398598 ) ) ;
#12014 = ORIENTED_EDGE ( 'NONE', *, *, #12527, .T. ) ;
#12015 = CARTESIAN_POINT ( 'NONE',  ( 2.237328452597175499, 7.708027139131397476, 31.02581378992296735 ) ) ;
#12016 = ORIENTED_EDGE ( 'NONE', *, *, #3083, .F. ) ;
#12018 = VERTEX_POINT ( 'NONE', #4376 ) ;
#12017 = DIRECTION ( 'NONE',  ( -1.000000000000000000, 0.000000000000000000, 0.000000000000000000 ) ) ;
#12019 = ORIENTED_EDGE ( 'NONE', *, *, #8796, .T. ) ;
#12020 = CARTESIAN_POINT ( 'NONE',  ( -20.61203582816999713, -107.2792658164648003, -6.701628977179171720 ) ) ;
#12021 = ORIENTED_EDGE ( 'NONE', *, *, #10337, .T. ) ;
#12022 = EDGE_CURVE ( 'NONE', #7911, #6717, #11318, .T. ) ;
#12023 = CARTESIAN_POINT ( 'NONE',  ( -15.49969986081099904, 20.99262100756200056, 24.21206422150099868 ) ) ;
#12024 =( BOUNDED_CURVE ( )  B_SPLINE_CURVE ( 3, ( #14684, #6784, #7936, #8787 ),
 .UNSPECIFIED., .F., .T. ) 
 B_SPLINE_CURVE_WITH_KNOTS ( ( 4, 4 ),
 ( 2.168404344971017989E-16, 1.513547814233613842 ),
 .UNSPECIFIED. ) 
 CURVE ( )  GEOMETRIC_REPRESENTATION_ITEM ( )  RATIONAL_B_SPLINE_CURVE ( ( 1.000000000000000000, 0.8180365063541268356, 0.8180365063541268356, 1.000000000000000000 ) ) 
 REPRESENTATION_ITEM ( '' )  );
#12025 = AXIS2_PLACEMENT_3D ( 'NONE', #5398, #5053, #4980 ) ;
#12026 = DIRECTION ( 'NONE',  ( 0.000000000000000000, 1.000000000000000000, 1.224646799147350002E-16 ) ) ;
#12027 = APPLICATION_PROTOCOL_DEFINITION ( 'draft international standard', 'automotive_design', 1998, #5084 ) ;
#12028 = DIRECTION ( 'NONE',  ( -8.018662683283438208E-16, 5.975035461963189015E-16, 1.000000000000000000 ) ) ;
#12029 = CYLINDRICAL_SURFACE ( 'NONE', #6885, 2.500000000000002220 ) ;
#12030 = AXIS2_PLACEMENT_3D ( 'NONE', #4889, #9542, #12075 ) ;
#12031 = DIRECTION ( 'NONE',  ( 0.5975035461963189576, 0.8018662683283437342, 0.000000000000000000 ) ) ;
#12032 = AXIS2_PLACEMENT_3D ( 'NONE', #10621, #1365, #13915 ) ;
#12033 = ORIENTED_EDGE ( 'NONE', *, *, #7434, .T. ) ;
#12034 = CARTESIAN_POINT ( 'NONE',  ( -5.650856670168516338, -15.08880645082409622, 54.00231026484399166 ) ) ;
#12035 = ORIENTED_EDGE ( 'NONE', *, *, #3908, .F. ) ;
#12036 = VERTEX_POINT ( 'NONE', #4447 ) ;
#12037 = AXIS2_PLACEMENT_3D ( 'NONE', #10717, #320, #8101 ) ;
#12038 = VECTOR ( 'NONE', #8550, 1000.000000000000000 ) ;
#12039 = LINE ( 'NONE', #10888, #12769 ) ;
#12040 = VERTEX_POINT ( 'NONE', #10407 ) ;
#12041 = ORIENTED_EDGE ( 'NONE', *, *, #1971, .T. ) ;
#12042 = CARTESIAN_POINT ( 'NONE',  ( -7.654212976755197850, -10.04550297615607768, 56.85231026484400019 ) ) ;
#12043 = EDGE_CURVE ( 'NONE', #10505, #11993, #1005, .T. ) ;
#12044 = EDGE_CURVE ( 'NONE', #2383, #11942, #11036, .T. ) ;
#12045 =( NAMED_UNIT ( * ) SI_UNIT ( $, .STERADIAN. ) SOLID_ANGLE_UNIT ( ) );
#12046 = DIRECTION ( 'NONE',  ( 0.1855175943453168941, 0.9826409426582662920, -4.383711467890769768E-16 ) ) ;
#12047 = CIRCLE ( 'NONE', #6162, 9.974999999999999645 ) ;
#12048 = CONICAL_SURFACE ( 'NONE', #11797, 0.9999999999999990008, 0.7853981633974476129 ) ;
#12049 = DIRECTION ( 'NONE',  ( 0.000000000000000000, -0.1872998510044090459, -0.9823027872370749813 ) ) ;
#12051 = CARTESIAN_POINT ( 'NONE',  ( -12.72810521832141362, -22.14910990341453001, 57.00231026484399166 ) ) ;
#12050 = DIRECTION ( 'NONE',  ( 8.018662683283438208E-16, -5.975035461963189015E-16, -1.000000000000000000 ) ) ;
#12052 = ORIENTED_EDGE ( 'NONE', *, *, #2963, .T. ) ;
#12053 = CARTESIAN_POINT ( 'NONE',  ( -15.49969986081099194, -52.50737899243800655, 11.50231026484399521 ) ) ;
#12054 = EDGE_LOOP ( 'NONE', ( #2473, #8915, #683, #11689 ) ) ;
#12055 = CARTESIAN_POINT ( 'NONE',  ( -15.49969986081099904, 37.56536188261469533, 24.21206422150100224 ) ) ;
#12056 = ORIENTED_EDGE ( 'NONE', *, *, #3966, .F. ) ;
#12057 = ORIENTED_EDGE ( 'NONE', *, *, #9107, .F. ) ;
#12058 = LINE ( 'NONE', #7672, #1512 ) ;
#12059 = ORIENTED_EDGE ( 'NONE', *, *, #2403, .F. ) ;
#12060 = VECTOR ( 'NONE', #1773, 1000.000000000000000 ) ;
#12061 = ADVANCED_FACE ( 'NONE', ( #1305 ), #13095, .T. ) ;
#12062 = AXIS2_PLACEMENT_3D ( 'NONE', #13663, #5469, #1811 ) ;
#12063 = EDGE_CURVE ( 'NONE', #14661, #12770, #10871, .T. ) ;
#12064 = ADVANCED_FACE ( 'NONE', ( #9412 ), #2382, .F. ) ;
#12065 = DIRECTION ( 'NONE',  ( 1.000000000000000000, 1.201369187114119994E-15, 9.616040805000176517E-16 ) ) ;
#12066 = DIRECTION ( 'NONE',  ( 0.000000000000000000, 0.000000000000000000, 1.000000000000000000 ) ) ;
#12067 = EDGE_CURVE ( 'NONE', #1451, #5453, #3904, .T. ) ;
#12068 = AXIS2_PLACEMENT_3D ( 'NONE', #11385, #1982, #12621 ) ;
#12069 = DIRECTION ( 'NONE',  ( 0.000000000000000000, 1.000000000000000000, 1.224646799147350002E-16 ) ) ;
#12070 = DIRECTION ( 'NONE',  ( 0.000000000000000000, 0.1872998510044689147, 0.9823027872370635460 ) ) ;
#12071 = ORIENTED_EDGE ( 'NONE', *, *, #9266, .F. ) ;
#12072 = DIRECTION ( 'NONE',  ( 0.1165201156931293391, 0.9931883319083343320, -4.999999999999998416E-16 ) ) ;
#12073 = CYLINDRICAL_SURFACE ( 'NONE', #2859, 10.00000000000000000 ) ;
#12074 = VERTEX_POINT ( 'NONE', #14239 ) ;
#12075 = DIRECTION ( 'NONE',  ( 0.000000000000000000, 1.224646799147350002E-16, -1.000000000000000000 ) ) ;
#12076 = ORIENTED_EDGE ( 'NONE', *, *, #1314, .F. ) ;
#12077 = EDGE_LOOP ( 'NONE', ( #7579, #7459, #5813, #5459 ) ) ;
#12078 = CARTESIAN_POINT ( 'NONE',  ( -15.57469986081567370, -23.50709773848280904, 57.00223526477360281 ) ) ;
#12079 = EDGE_CURVE ( 'NONE', #1553, #8640, #8375, .T. ) ;
#12080 = EDGE_CURVE ( 'NONE', #12967, #1536, #1309, .T. ) ;
#12081 = CIRCLE ( 'NONE', #4747, 1.744527686444488968 ) ;
#12082 = PLANE ( 'NONE',  #8356 ) ;
#12083 = CARTESIAN_POINT ( 'NONE',  ( -7.499960972858382924, -49.00661531336379539, 19.43850304437339460 ) ) ;
#12084 = AXIS2_PLACEMENT_3D ( 'NONE', #353, #3783, #4784 ) ;
#12085 = CARTESIAN_POINT ( 'NONE',  ( 14.70471644742069373, -27.47017211369107770, 1.987150903830744664 ) ) ;
#12086 = CARTESIAN_POINT ( 'NONE',  ( -23.08034316846174150, -10.72437754756471762, 57.00231026484397745 ) ) ;
#12087 = EDGE_LOOP ( 'NONE', ( #5980, #6813, #14064, #11494 ) ) ;
#12088 = CARTESIAN_POINT ( 'NONE',  ( -24.39712111458419130, -18.01698208283363556, 57.00231026484397745 ) ) ;
#12089 = CARTESIAN_POINT ( 'NONE',  ( -33.53940702758666248, -41.28381732916982827, 52.37824589759239302 ) ) ;
#12090 = AXIS2_PLACEMENT_3D ( 'NONE', #2143, #11321, #10159 ) ;
#12091 = ORIENTED_EDGE ( 'NONE', *, *, #3908, .T. ) ;
#12092 = CARTESIAN_POINT ( 'NONE',  ( -7.512805849530849400, -44.04964101872660365, -5.039951761444699585 ) ) ;
#12093 = ORIENTED_EDGE ( 'NONE', *, *, #6544, .F. ) ;
#12095 = ORIENTED_EDGE ( 'NONE', *, *, #6770, .T. ) ;
#12094 = CARTESIAN_POINT ( 'NONE',  ( -36.64373166576667273, -37.36437517128344155, -11.46837648659897546 ) ) ;
#12096 = EDGE_LOOP ( 'NONE', ( #6915, #1926, #2432, #9106, #3150, #14794, #5125, #6138, #4085, #7072, #1511, #3072, #5705, #4967, #4792, #3681, #7539, #11387, #15091, #4526, #8274, #9871, #8262, #13249, #3063, #10211, #7091, #3997, #1345, #6031, #9162, #9465, #9793, #11687, #12364, #9426, #6956, #6328, #13409, #291, #12739, #5940, #4310, #943, #14940, #8614, #6405, #1889, #4850, #4337, #12482, #956, #8185, #8883, #8933, #11613, #11615, #4617, #2349, #6160, #10042, #14230, #870, #2097, #6202, #13671, #294, #5966, #4468, #6893, #6312, #6671, #13762, #11010, #12818, #5749, #4240, #14961, #502, #14457, #8506, #629, #10074, #9775, #4940, #188, #2895, #13002, #14667, #7926, #9120, #6964 ) ) ;
#12097 = LINE ( 'NONE', #8711, #6150 ) ;
#12098 = DIRECTION ( 'NONE',  ( 1.000000000000000000, 1.201369187114119994E-15, 9.616040805000176517E-16 ) ) ;
#12099 = DIRECTION ( 'NONE',  ( 1.000000000000000000, 1.201369187114119994E-15, 9.616040805000176517E-16 ) ) ;
#12100 = VECTOR ( 'NONE', #11791, 1000.000000000000000 ) ;
#12101 = CARTESIAN_POINT ( 'NONE',  ( -14.84599537932207802, -3.507399398443247662, 61.71206405750629642 ) ) ;
#12102 = DIRECTION ( 'NONE',  ( 0.000000000000000000, 0.000000000000000000, -1.000000000000000000 ) ) ;
#12103 = EDGE_CURVE ( 'NONE', #7229, #13194, #2769, .T. ) ;
#12104 = ADVANCED_FACE ( 'NONE', ( #11941, #168 ), #9489, .F. ) ;
#12105 = LINE ( 'NONE', #5211, #3732 ) ;
#12106 = DIRECTION ( 'NONE',  ( -0.5975035461963187355, -0.8018662683283439563, 0.000000000000000000 ) ) ;
#12107 = ORIENTED_EDGE ( 'NONE', *, *, #6289, .F. ) ;
#12108 = CARTESIAN_POINT ( 'NONE',  ( -15.19690733689918183, -23.47778227853769550, 54.00231026484399166 ) ) ;
#12109 = ORIENTED_EDGE ( 'NONE', *, *, #14124, .T. ) ;
#12110 = ORIENTED_EDGE ( 'NONE', *, *, #11167, .F. ) ;
#12111 = CARTESIAN_POINT ( 'NONE',  ( -17.95685260396766125, -23.17500669507537836, 56.85231026484400019 ) ) ;
#12112 = VERTEX_POINT ( 'NONE', #5055 ) ;
#12113 = CARTESIAN_POINT ( 'NONE',  ( 7.200737182676100190, 4.873818854045000037, 27.91208557747711083 ) ) ;
#12114 = FACE_OUTER_BOUND ( 'NONE', #394, .T. ) ;
#12115 = CARTESIAN_POINT ( 'NONE',  ( 2.500300139188999182, -51.00737899243799944, -13.39525803434800011 ) ) ;
#12116 = VECTOR ( 'NONE', #2281, 1000.000000000000114 ) ;
#12117 = CARTESIAN_POINT ( 'NONE',  ( -38.36664365575047952, 4.365428709180945610, 21.66608770973884646 ) ) ;
#12118 = ADVANCED_FACE ( 'NONE', ( #1459 ), #88, .T. ) ;
#12120 = CARTESIAN_POINT ( 'NONE',  ( -35.91308956371933192, 5.973563155936505886, 18.89224887993488977 ) ) ;
#12119 = CARTESIAN_POINT ( 'NONE',  ( -15.49969986081099904, 70.89785811302749607, 24.21206422150100579 ) ) ;
#12121 = ORIENTED_EDGE ( 'NONE', *, *, #1824, .T. ) ;
#12122 = CARTESIAN_POINT ( 'NONE',  ( -12.60362876103445373, -23.05271278361805543, 56.85231026484400019 ) ) ;
#12123 = ORIENTED_EDGE ( 'NONE', *, *, #5579, .T. ) ;
#12124 = CARTESIAN_POINT ( 'NONE',  ( -21.29301345516119071, -7.881655252552254964, 56.85231026484398598 ) ) ;
#12125 = ORIENTED_EDGE ( 'NONE', *, *, #2861, .T. ) ;
#12126 = ORIENTED_EDGE ( 'NONE', *, *, #5360, .F. ) ;
#12127 = DIRECTION ( 'NONE',  ( 0.000000000000000000, 0.1872998510044689147, 0.9823027872370635460 ) ) ;
#12128 = ORIENTED_EDGE ( 'NONE', *, *, #3365, .F. ) ;
#12129 = AXIS2_PLACEMENT_3D ( 'NONE', #11620, #4744, #12942 ) ;
#12130 = CARTESIAN_POINT ( 'NONE',  ( 4.893136743221020879, 5.983413651705625114, 18.88106025385081566 ) ) ;
#12131 = CARTESIAN_POINT ( 'NONE',  ( -20.82326471215695562, -106.0804592893369147, -6.239094581732940625 ) ) ;
#12132 = CARTESIAN_POINT ( 'NONE',  ( -11.30912773046065922, -22.58799119088164886, 56.76750275176264182 ) ) ;
#12133 = DIRECTION ( 'NONE',  ( -8.018662683283438208E-16, 5.975035461963189015E-16, 1.000000000000000000 ) ) ;
#12134 = EDGE_CURVE ( 'NONE', #3679, #1866, #8334, .T. ) ;
#12135 = DIRECTION ( 'NONE',  ( 0.3533329742249663452, 0.9354976265738675911, -2.756373558169968730E-16 ) ) ;
#12136 = ORIENTED_EDGE ( 'NONE', *, *, #6658, .T. ) ;
#12137 = DIRECTION ( 'NONE',  ( -0.9578660637129379207, 0.2872152572324145892, -9.396926207859088029E-16 ) ) ;
#12138 = VECTOR ( 'NONE', #3590, 1000.000000000000000 ) ;
#12139 = DIRECTION ( 'NONE',  ( 8.018662683283438208E-16, -5.975035461963189015E-16, -1.000000000000000000 ) ) ;
#12140 = EDGE_LOOP ( 'NONE', ( #8045, #14781, #8259, #4451 ) ) ;
#12141 = EDGE_CURVE ( 'NONE', #221, #11420, #3680, .T. ) ;
#12142 = CARTESIAN_POINT ( 'NONE',  ( 21.98622857737163727, -23.92291445542225858, 23.16614582331327554 ) ) ;
#12143 = ORIENTED_EDGE ( 'NONE', *, *, #8205, .F. ) ;
#12144 = DIRECTION ( 'NONE',  ( -8.018662683283438208E-16, 5.975035461963189015E-16, 1.000000000000000000 ) ) ;
#12145 = ORIENTED_EDGE ( 'NONE', *, *, #8493, .F. ) ;
#12146 = CIRCLE ( 'NONE', #5537, 2.999999999999999112 ) ;
#12147 = AXIS2_PLACEMENT_3D ( 'NONE', #3803, #1658, #1358 ) ;
#12148 = DIRECTION ( 'NONE',  ( 0.000000000000000000, 0.000000000000000000, 1.000000000000000000 ) ) ;
#12149 = AXIS2_PLACEMENT_3D ( 'NONE', #7073, #3575, #14365 ) ;
#12150 = CARTESIAN_POINT ( 'NONE',  ( -7.671650320578238258, -48.38766871647332835, 17.85456079179654765 ) ) ;
#12151 = CARTESIAN_POINT ( 'NONE',  ( 17.94160745424604642, -29.55396020057183648, 7.242669092553135179 ) ) ;
#12152 = EDGE_CURVE ( 'NONE', #2093, #3246, #10558, .T. ) ;
#12153 = DIRECTION ( 'NONE',  ( -0.8543800322332368857, -0.5196486895212314439, -3.746065934159101186E-16 ) ) ;
#12154 = VERTEX_POINT ( 'NONE', #10790 ) ;
#12155 = CARTESIAN_POINT ( 'NONE',  ( -9.499699860810959962, -67.00737899243799234, -5.497689735155993240 ) ) ;
#12156 = EDGE_CURVE ( 'NONE', #10535, #11202, #92, .T. ) ;
#12157 = CARTESIAN_POINT ( 'NONE',  ( -33.99488797801397055, -39.83604612059843930, 52.12407946957260663 ) ) ;
#12158 = EDGE_CURVE ( 'NONE', #8821, #11659, #2529, .T. ) ;
#12159 = ORIENTED_EDGE ( 'NONE', *, *, #3571, .F. ) ;
#12160 = ORIENTED_EDGE ( 'NONE', *, *, #8847, .F. ) ;
#12161 = CIRCLE ( 'NONE', #7754, 4.999999999999999112 ) ;
#12162 = VECTOR ( 'NONE', #14937, 1000.000000000000000 ) ;
#12164 = ORIENTED_EDGE ( 'NONE', *, *, #515, .F. ) ;
#12163 = CARTESIAN_POINT ( 'NONE',  ( -33.88323046362949498, -40.08477038825456873, -13.18250565558182785 ) ) ;
#12165 = EDGE_LOOP ( 'NONE', ( #4643, #10979, #11901, #9190 ) ) ;
#12166 = VECTOR ( 'NONE', #9179, 1000.000000000000000 ) ;
#12167 = DIRECTION ( 'NONE',  ( -1.169602638241520408E-15, 0.1872998510044540654, 0.9823027872370663216 ) ) ;
#12168 = CARTESIAN_POINT ( 'NONE',  ( -15.53979317422733786, -13.47750381512840967, 56.85231026484398598 ) ) ;
#12169 = CARTESIAN_POINT ( 'NONE',  ( -33.01292635343269666, 8.758714366253697037, 16.84401747001000160 ) ) ;
#12170 = CARTESIAN_POINT ( 'NONE',  ( -7.758527451664997798, -48.50737899243800655, -5.497689735156000346 ) ) ;
#12171 = DIRECTION ( 'NONE',  ( -0.7032868978765923762, -0.7109061395677488404, -1.391731009600549731E-16 ) ) ;
#12172 = CARTESIAN_POINT ( 'NONE',  ( -15.50552586659557797, -13.55703840903364288, 56.85231026484398598 ) ) ;
#12173 = AXIS2_PLACEMENT_3D ( 'NONE', #11510, #4479, #9133 ) ;
#12174 = EDGE_CURVE ( 'NONE', #2842, #2678, #1476, .T. ) ;
#12175 = EDGE_CURVE ( 'NONE', #8446, #11671, #2266, .T. ) ;
#12176 = CARTESIAN_POINT ( 'NONE',  ( -15.49969986081099194, -57.00737899243800655, 19.50231026484398811 ) ) ;
#12177 = ORIENTED_EDGE ( 'NONE', *, *, #7, .T. ) ;
#12178 = EDGE_CURVE ( 'NONE', #11708, #4294, #4127, .T. ) ;
#12179 = DIRECTION ( 'NONE',  ( 0.000000000000000000, 9.130123557772668334E-17, -1.000000000000000000 ) ) ;
#12180 = ORIENTED_EDGE ( 'NONE', *, *, #4388, .F. ) ;
#12181 = LINE ( 'NONE', #14551, #10728 ) ;
#12182 = EDGE_LOOP ( 'NONE', ( #3035, #11918 ) ) ;
#12183 = ORIENTED_EDGE ( 'NONE', *, *, #3359, .T. ) ;
#12184 = CIRCLE ( 'NONE', #8015, 9.974999999999999645 ) ;
#12185 = DIRECTION ( 'NONE',  ( 5.000000000000000389E-16, -0.4999999999999998890, 0.8660254037844387076 ) ) ;
#12186 = ORIENTED_EDGE ( 'NONE', *, *, #16, .T. ) ;
#12187 = DIRECTION ( 'NONE',  ( 8.018662683283438208E-16, -5.975035461963189015E-16, -1.000000000000000000 ) ) ;
#12188 = CIRCLE ( 'NONE', #9237, 3.250000000000002665 ) ;
#12189 = EDGE_CURVE ( 'NONE', #11256, #3447, #1053, .T. ) ;
#12190 = DIRECTION ( 'NONE',  ( 8.018662683283438208E-16, -5.975035461963189015E-16, -1.000000000000000000 ) ) ;
#12191 = CARTESIAN_POINT ( 'NONE',  ( 13.85920135429429934, -27.00737899243800300, 39.96206422150099513 ) ) ;
#12192 = CIRCLE ( 'NONE', #5582, 9.974999999999999645 ) ;
#12193 = AXIS2_PLACEMENT_3D ( 'NONE', #8846, #3114, #10879 ) ;
#12195 = LINE ( 'NONE', #1710, #15005 ) ;
#12194 = FACE_OUTER_BOUND ( 'NONE', #1382, .T. ) ;
#12196 = ORIENTED_EDGE ( 'NONE', *, *, #1118, .F. ) ;
#12197 = CARTESIAN_POINT ( 'NONE',  ( 9.000300139189000959, -32.00737899243799944, 24.21206422150099868 ) ) ;
#12198 = EDGE_LOOP ( 'NONE', ( #4603, #13000, #3464, #13876 ) ) ;
#12199 = DIRECTION ( 'NONE',  ( 0.000000000000000000, 0.000000000000000000, 1.000000000000000000 ) ) ;
#12200 = ORIENTED_EDGE ( 'NONE', *, *, #14035, .F. ) ;
#12201 = EDGE_LOOP ( 'NONE', ( #4908, #5290, #798, #10405, #755, #9697 ) ) ;
#12202 = LINE ( 'NONE', #8745, #1279 ) ;
#12203 = CARTESIAN_POINT ( 'NONE',  ( -15.49969986081099904, 22.99262100756200056, 24.21206422150100224 ) ) ;
#12204 = EDGE_LOOP ( 'NONE', ( #10917, #5345, #7045, #7741 ) ) ;
#12205 = AXIS2_PLACEMENT_3D ( 'NONE', #13066, #6076, #7304 ) ;
#12206 = CARTESIAN_POINT ( 'NONE',  ( -15.61203582816999891, -107.9196643519486969, -5.433976602192394090 ) ) ;
#12207 = EDGE_CURVE ( 'NONE', #1735, #11004, #4051, .T. ) ;
#12208 = CARTESIAN_POINT ( 'NONE',  ( -15.49969986081099727, 71.39262100756199914, 32.52626782222684909 ) ) ;
#12209 = FACE_OUTER_BOUND ( 'NONE', #1098, .T. ) ;
#12210 = CARTESIAN_POINT ( 'NONE',  ( -15.24029490235350259, -21.57855976525750563, 57.00231026484399166 ) ) ;
#12211 = CIRCLE ( 'NONE', #8292, 15.62500000000000000 ) ;
#12212 = DIRECTION ( 'NONE',  ( 1.000000000000000000, 0.000000000000000000, 0.000000000000000000 ) ) ;
#12213 = CARTESIAN_POINT ( 'NONE',  ( -2.216578225681298697, -31.14135358865350511, -123.9247733198440073 ) ) ;
#12214 = VERTEX_POINT ( 'NONE', #5126 ) ;
#12215 = DIRECTION ( 'NONE',  ( 0.1165201156931293391, 0.9931883319083343320, -4.999999999999998416E-16 ) ) ;
#12216 = ADVANCED_FACE ( 'NONE', ( #7559 ), #3049, .F. ) ;
#12217 = LINE ( 'NONE', #5254, #10722 ) ;
#12218 = ORIENTED_EDGE ( 'NONE', *, *, #12158, .T. ) ;
#12219 = AXIS2_PLACEMENT_3D ( 'NONE', #14878, #4400, #4475 ) ;
#12220 = CARTESIAN_POINT ( 'NONE',  ( 22.00030675015428727, -23.75730271206433386, 24.00114908445582529 ) ) ;
#12221 = CARTESIAN_POINT ( 'NONE',  ( -14.60940909295887913, -15.57374835648654532, 51.00231026484399166 ) ) ;
#12222 = ORIENTED_EDGE ( 'NONE', *, *, #2479, .T. ) ;
#12223 = CARTESIAN_POINT ( 'NONE',  ( -31.57904533557010751, -52.92803351767889097, 53.45077026338344695 ) ) ;
#12224 = ORIENTED_EDGE ( 'NONE', *, *, #8722, .F. ) ;
#12225 = CARTESIAN_POINT ( 'NONE',  ( -15.49969986081099904, -27.00737899243799944, -5.497689735156000346 ) ) ;
#12226 = B_SPLINE_CURVE_WITH_KNOTS ( 'NONE', 3,
 ( #26, #9499, #11951, #8191, #4919, #3612, #2691, #14172, #13108, #4994, #5892, #4764, #9653, #14324, #331, #9421, #3836, #6042 ),
 .UNSPECIFIED., .F., .F.,
 ( 4, 2, 2, 2, 2, 2, 2, 2, 4 ),
 ( 0.000000000000000000, 0.0008864497783454140366, 0.001772899556690828073, 0.002659349335036241893, 0.003545799113381656147, 0.004432248891727070400, 0.005318698670072483786, 0.006205148448417898040, 0.007091598226763312293 ),
 .UNSPECIFIED. ) ;
#12227 = ADVANCED_FACE ( 'NONE', ( #681 ), #13324, .F. ) ;
#12228 = DIRECTION ( 'NONE',  ( 0.000000000000000000, 0.000000000000000000, -1.000000000000000000 ) ) ;
#12229 = ADVANCED_FACE ( 'NONE', ( #4201 ), #11009, .T. ) ;
#12230 = CARTESIAN_POINT ( 'NONE',  ( -15.49969986081099904, 71.39262100756199914, 24.21206422150100579 ) ) ;
#12231 = AXIS2_PLACEMENT_3D ( 'NONE', #12417, #11567, #10182 ) ;
#12232 = DIRECTION ( 'NONE',  ( -8.018662683283438208E-16, 5.975035461963189015E-16, 1.000000000000000000 ) ) ;
#12233 = DIRECTION ( 'NONE',  ( 0.000000000000000000, 1.224646799147350002E-16, -1.000000000000000000 ) ) ;
#12234 = ORIENTED_EDGE ( 'NONE', *, *, #6951, .T. ) ;
#12235 = FACE_OUTER_BOUND ( 'NONE', #8523, .T. ) ;
#12236 = CARTESIAN_POINT ( 'NONE',  ( -7.758527451665001351, -44.50737899243799944, -5.497689735156000346 ) ) ;
#12237 = ORIENTED_EDGE ( 'NONE', *, *, #3956, .F. ) ;
#12238 = ORIENTED_EDGE ( 'NONE', *, *, #12962, .T. ) ;
#12240 = VERTEX_POINT ( 'NONE', #14758 ) ;
#12239 = CARTESIAN_POINT ( 'NONE',  ( -36.69937278055155616, -37.34275670915150869, -11.43026766154685703 ) ) ;
#12241 = VERTEX_POINT ( 'NONE', #5417 ) ;
#12242 = CARTESIAN_POINT ( 'NONE',  ( -2.216578225681298697, -31.14135358865360104, 59.28069236156870403 ) ) ;
#12243 = FACE_OUTER_BOUND ( 'NONE', #14179, .T. ) ;
#12244 = EDGE_CURVE ( 'NONE', #3602, #6022, #11240, .T. ) ;
#12245 = DIRECTION ( 'NONE',  ( 8.018662683283438208E-16, -5.975035461963189015E-16, -1.000000000000000000 ) ) ;
#12246 = ADVANCED_FACE ( 'NONE', ( #9792 ), #3979, .T. ) ;
#12247 = DIRECTION ( 'NONE',  ( -8.018662683283438208E-16, 5.975035461963189015E-16, 1.000000000000000000 ) ) ;
#12248 = EDGE_CURVE ( 'NONE', #5768, #5839, #10340, .T. ) ;
#12249 = DIRECTION ( 'NONE',  ( 0.000000000000000000, 0.000000000000000000, -1.000000000000000000 ) ) ;
#12250 = DIRECTION ( 'NONE',  ( 0.8018662683283436232, -0.5975035461963189576, 9.999999999999998805E-16 ) ) ;
#12251 = VECTOR ( 'NONE', #7517, 1000.000000000000000 ) ;
#12252 = LINE ( 'NONE', #6565, #9683 ) ;
#12253 = EDGE_CURVE ( 'NONE', #8358, #8353, #4021, .T. ) ;
#12254 = CARTESIAN_POINT ( 'NONE',  ( -15.86970092169881141, -16.66117552174622318, 57.00231026484397745 ) ) ;
#12255 = CARTESIAN_POINT ( 'NONE',  ( -12.98295438134161195, -5.834228258119843247, 56.85231026484398598 ) ) ;
#12256 = ORIENTED_EDGE ( 'NONE', *, *, #9844, .F. ) ;
#12257 = FACE_OUTER_BOUND ( 'NONE', #7406, .T. ) ;
#12259 = VERTEX_POINT ( 'NONE', #12466 ) ;
#12258 = CARTESIAN_POINT ( 'NONE',  ( -15.49969986081099904, 71.39262100756199914, 15.89786062077516782 ) ) ;
#12260 = ORIENTED_EDGE ( 'NONE', *, *, #2818, .T. ) ;
#12261 = CARTESIAN_POINT ( 'NONE',  ( -20.61203582816999713, -106.9749035585825681, -5.105386947918939988 ) ) ;
#12263 = ORIENTED_EDGE ( 'NONE', *, *, #9386, .F. ) ;
#12262 = FACE_OUTER_BOUND ( 'NONE', #8830, .T. ) ;
#12264 = VECTOR ( 'NONE', #5959, 1000.000000000000114 ) ;
#12265 = CARTESIAN_POINT ( 'NONE',  ( -13.50277480631462979, -9.463945884570895473, -13.23572242406894617 ) ) ;
#12266 = EDGE_CURVE ( 'NONE', #6717, #9043, #12806, .T. ) ;
#12267 = CARTESIAN_POINT ( 'NONE',  ( -14.07534335717186202, -5.558639560896826204, 57.00231026484397745 ) ) ;
#12268 = LINE ( 'NONE', #1706, #9975 ) ;
#12269 = VECTOR ( 'NONE', #9358, 999.9999999999998863 ) ;
#12270 = VECTOR ( 'NONE', #2906, 1000.000000000000000 ) ;
#12271 = VECTOR ( 'NONE', #12376, 1000.000000000000000 ) ;
#12273 = DIRECTION ( 'NONE',  ( -8.018662683283438208E-16, 5.975035461963189015E-16, 1.000000000000000000 ) ) ;
#12272 = FACE_OUTER_BOUND ( 'NONE', #2326, .T. ) ;
#12274 = EDGE_LOOP ( 'NONE', ( #8540, #416, #14983, #5348, #11314, #1047, #11268, #9276, #3048 ) ) ;
#12275 = PLANE ( 'NONE',  #12414 ) ;
#12276 = ORIENTED_EDGE ( 'NONE', *, *, #10140, .T. ) ;
#12277 = DIRECTION ( 'NONE',  ( -8.018662683283438208E-16, 5.975035461963189015E-16, 1.000000000000000000 ) ) ;
#12278 = VERTEX_POINT ( 'NONE', #4358 ) ;
#12279 = ORIENTED_EDGE ( 'NONE', *, *, #14636, .F. ) ;
#12280 = CARTESIAN_POINT ( 'NONE',  ( 21.85920135429435263, -27.21949063834600935, 20.96206422150100224 ) ) ;
#12281 = EDGE_CURVE ( 'NONE', #2152, #4803, #2543, .T. ) ;
#12282 = CARTESIAN_POINT ( 'NONE',  ( -15.49969986081099904, 7.183219930803497633, 24.21206422150099868 ) ) ;
#12283 = ORIENTED_EDGE ( 'NONE', *, *, #3536, .T. ) ;
#12284 = DIRECTION ( 'NONE',  ( 1.000000000000000000, 0.000000000000000000, 0.000000000000000000 ) ) ;
#12285 = VECTOR ( 'NONE', #6933, 1000.000000000000000 ) ;
#12286 = VECTOR ( 'NONE', #8797, 1000.000000000000114 ) ;
#12287 = CARTESIAN_POINT ( 'NONE',  ( 4.742609669324512112, 6.055639158887895945, 18.80100070848684624 ) ) ;
#12288 = CARTESIAN_POINT ( 'NONE',  ( -22.00391959472895209, -7.178368354675633611, 56.85231026484398598 ) ) ;
#12289 = DIRECTION ( 'NONE',  ( -1.224646799147350002E-16, -1.224646799147350002E-16, 1.000000000000000000 ) ) ;
#12290 = LINE ( 'NONE', #1810, #13536 ) ;
#12291 = DIRECTION ( 'NONE',  ( -0.9931883319083342210, 0.1165201156931306992, 0.000000000000000000 ) ) ;
#12292 = ORIENTED_EDGE ( 'NONE', *, *, #11117, .F. ) ;
#12293 = CARTESIAN_POINT ( 'NONE',  ( -15.09158957740191731, -107.1622034095870077, -6.087689735156000204 ) ) ;
#12294 = ADVANCED_FACE ( 'NONE', ( #8934 ), #5642, .F. ) ;
#12295 = VERTEX_POINT ( 'NONE', #3203 ) ;
#12296 = ADVANCED_FACE ( 'NONE', ( #4581 ), #2211, .F. ) ;
#12297 = AXIS2_PLACEMENT_3D ( 'NONE', #8727, #10961, #7650 ) ;
#12298 = DIRECTION ( 'NONE',  ( 0.5975035461963187355, 0.8018662683283439563, 0.000000000000000000 ) ) ;
#12299 = DIRECTION ( 'NONE',  ( -0.7582332219680880669, 0.6519834208811540188, -9.975640502598240034E-16 ) ) ;
#12300 = ORIENTED_EDGE ( 'NONE', *, *, #4513, .T. ) ;
#12301 = DIRECTION ( 'NONE',  ( 0.5975035461963189576, 0.8018662683283437342, 0.000000000000000000 ) ) ;
#12302 = CARTESIAN_POINT ( 'NONE',  ( -35.49969986081099904, -19.50737899243800300, -7.509379629622798369 ) ) ;
#12303 = CIRCLE ( 'NONE', #8873, 9.974999999999999645 ) ;
#12304 = CARTESIAN_POINT ( 'NONE',  ( -1.508527451664997798, -47.80641709811465034, -6.247689735156000346 ) ) ;
#12305 = CIRCLE ( 'NONE', #822, 9.974999999999999645 ) ;
#12306 = DIRECTION ( 'NONE',  ( 0.5975035461963187355, 0.8018662683283439563, 0.000000000000000000 ) ) ;
#12307 = CARTESIAN_POINT ( 'NONE',  ( 4.500300139189000959, -19.50737899243801010, -7.509379629622798369 ) ) ;
#12308 = ORIENTED_EDGE ( 'NONE', *, *, #1501, .F. ) ;
#12309 = CARTESIAN_POINT ( 'NONE',  ( -32.93478177869805279, 9.209028802409704895, 31.76314389137934668 ) ) ;
#12310 = DIRECTION ( 'NONE',  ( 8.018662683283438208E-16, -5.975035461963189015E-16, -1.000000000000000000 ) ) ;
#12311 = EDGE_CURVE ( 'NONE', #9278, #13407, #6856, .T. ) ;
#12312 = ORIENTED_EDGE ( 'NONE', *, *, #2986, .T. ) ;
#12314 = ORIENTED_EDGE ( 'NONE', *, *, #2278, .T. ) ;
#12313 = DIRECTION ( 'NONE',  ( 0.000000000000000000, 1.850371707708594316E-16, -1.000000000000000000 ) ) ;
#12315 = VERTEX_POINT ( 'NONE', #2289 ) ;
#12316 = PRESENTATION_LAYER_ASSIGNMENT (  '', '', ( #842 ) ) ;
#12317 = LINE ( 'NONE', #14911, #1525 ) ;
#12318 = ORIENTED_EDGE ( 'NONE', *, *, #6744, .F. ) ;
#12319 =( REPRESENTATION_RELATIONSHIP ('NONE','NONE', #2372, #6151 ) REPRESENTATION_RELATIONSHIP_WITH_TRANSFORMATION ( #11300 )SHAPE_REPRESENTATION_RELATIONSHIP( ) );
#12320 = CARTESIAN_POINT ( 'NONE',  ( -15.61203582816999891, -108.0739289917895007, -5.561265332623595015 ) ) ;
#12321 = LINE ( 'NONE', #11471, #3294 ) ;
#12322 = AXIS2_PLACEMENT_3D ( 'NONE', #7289, #9518, #14189 ) ;
#12323 = DIRECTION ( 'NONE',  ( -2.526242637138179679E-48, -1.000000000000000000, -1.224646799147350002E-16 ) ) ;
#12324 = CARTESIAN_POINT ( 'NONE',  ( -16.24959055444668365, -20.54292544936667397, 56.85231026484400019 ) ) ;
#12325 = AXIS2_PLACEMENT_3D ( 'NONE', #4121, #2052, #12381 ) ;
#12326 = CARTESIAN_POINT ( 'NONE',  ( -5.499699860811000818, -46.50737899243799944, 19.50231026484399877 ) ) ;
#12327 = DIRECTION ( 'NONE',  ( -0.9183863840214729901, -0.3956847857120157075, -4.999999999999999402E-16 ) ) ;
#12328 = EDGE_CURVE ( 'NONE', #13264, #5925, #10151, .T. ) ;
#12329 = CARTESIAN_POINT ( 'NONE',  ( -27.49969986081100259, -57.00737899243800655, 19.50231026484398811 ) ) ;
#12330 = EDGE_LOOP ( 'NONE', ( #10694, #9291, #14027, #4039 ) ) ;
#12331 = DIRECTION ( 'NONE',  ( 0.7109061395677416240, -0.7032868978765995926, 9.902680687415702019E-16 ) ) ;
#12333 = VERTEX_POINT ( 'NONE', #7849 ) ;
#12332 = DIRECTION ( 'NONE',  ( 1.366025403784438385E-15, -0.8910065241883674547, -0.4539904997395473596 ) ) ;
#12334 = ORIENTED_EDGE ( 'NONE', *, *, #12759, .F. ) ;
#12335 = EDGE_CURVE ( 'NONE', #11004, #13213, #11206, .T. ) ;
#12336 = CARTESIAN_POINT ( 'NONE',  ( -6.517576446443361426, -14.80457171870128974, 56.85231026484400019 ) ) ;
#12338 = ORIENTED_EDGE ( 'NONE', *, *, #3387, .F. ) ;
#12337 = CYLINDRICAL_SURFACE ( 'NONE', #13067, 8.000000000000000000 ) ;
#12339 = CARTESIAN_POINT ( 'NONE',  ( -22.53804163936502647, -6.438972523632135569, 57.00231026484397745 ) ) ;
#12340 = MECHANICAL_DESIGN_GEOMETRIC_PRESENTATION_REPRESENTATION (  '', ( #15019 ), #10376 ) ;
#12341 = ADVANCED_FACE ( 'NONE', ( #14982 ), #13761, .T. ) ;
#12342 = CARTESIAN_POINT ( 'NONE',  ( -15.49969986081098838, -17.75737899243799944, 54.00231026484400587 ) ) ;
#12343 = CARTESIAN_POINT ( 'NONE',  ( -15.61203582817000068, -106.1798807882712765, -5.562105325730672511 ) ) ;
#12344 = CARTESIAN_POINT ( 'NONE',  ( -7.804240102366930998, -47.71020347972489617, -7.689478587326622261 ) ) ;
#12345 = DIRECTION ( 'NONE',  ( -0.3190779711151160991, -0.04960027561187737438, -0.9464296386991939425 ) ) ;
#12346 = EDGE_CURVE ( 'NONE', #4983, #5733, #4507, .T. ) ;
#12347 = EDGE_LOOP ( 'NONE', ( #2699, #803, #9506, #12866, #14103, #14884, #2189, #7667, #6098, #3737 ) ) ;
#12348 = CARTESIAN_POINT ( 'NONE',  ( -13.02562488396841900, -21.19439421350821817, 56.85231026484400019 ) ) ;
#12349 = ADVANCED_FACE ( 'NONE', ( #9235 ), #13838, .F. ) ;
#12350 = ORIENTED_EDGE ( 'NONE', *, *, #1447, .T. ) ;
#12351 = CARTESIAN_POINT ( 'NONE',  ( -7.821737630532772378, -18.34578224045527151, 56.85231026484400019 ) ) ;
#12352 = ORIENTED_EDGE ( 'NONE', *, *, #1799, .F. ) ;
#12353 = ORIENTED_EDGE ( 'NONE', *, *, #2073, .T. ) ;
#12354 = ADVANCED_FACE ( 'NONE', ( #15057 ), #149, .F. ) ;
#12355 = CARTESIAN_POINT ( 'NONE',  ( -22.00675222451046409, -49.16858233193156735, 56.43373460882509818 ) ) ;
#12356 = VERTEX_POINT ( 'NONE', #5862 ) ;
#12357 = CARTESIAN_POINT ( 'NONE',  ( -23.43263029221230198, -15.01730109988151440, 56.85231026484398598 ) ) ;
#12358 = CARTESIAN_POINT ( 'NONE',  ( 4.814653393906814571, 6.021066563893142209, 18.83900906337587600 ) ) ;
#12359 = DIRECTION ( 'NONE',  ( 0.000000000000000000, 0.000000000000000000, -1.000000000000000000 ) ) ;
#12360 = VECTOR ( 'NONE', #141, 1000.000000000000000 ) ;
#12361 = DIRECTION ( 'NONE',  ( -8.018662683283438208E-16, 5.975035461963189015E-16, 1.000000000000000000 ) ) ;
#12362 = DIRECTION ( 'NONE',  ( 0.000000000000000000, -1.000000000000000000, -1.224646799147350002E-16 ) ) ;
#12363 = CYLINDRICAL_SURFACE ( 'NONE', #9820, 0.2499999999999997502 ) ;
#12364 = ORIENTED_EDGE ( 'NONE', *, *, #4767, .F. ) ;
#12365 = CARTESIAN_POINT ( 'NONE',  ( -15.61203582817000068, -106.2173407584721616, -5.758565883178085265 ) ) ;
#12366 = EDGE_CURVE ( 'NONE', #11542, #10768, #11568, .T. ) ;
#12367 = DIRECTION ( 'NONE',  ( 8.018662683283438208E-16, -5.975035461963189015E-16, -1.000000000000000000 ) ) ;
#12368 = ORIENTED_EDGE ( 'NONE', *, *, #5160, .T. ) ;
#12369 = CARTESIAN_POINT ( 'NONE',  ( 2.054681262915651008, 8.544173770627839559, 31.48152205384135982 ) ) ;
#12370 = EDGE_CURVE ( 'NONE', #10814, #1247, #4892, .T. ) ;
#12371 = PLANE ( 'NONE',  #1523 ) ;
#12372 = VECTOR ( 'NONE', #9169, 1000.000000000000000 ) ;
#12373 = CARTESIAN_POINT ( 'NONE',  ( -23.96284084890188382, -10.23071992935364527, 56.85231026484398598 ) ) ;
#12374 = ORIENTED_EDGE ( 'NONE', *, *, #6574, .T. ) ;
#12375 = DIRECTION ( 'NONE',  ( 0.5975035461963188466, 0.8018662683283437342, 0.000000000000000000 ) ) ;
#12376 = DIRECTION ( 'NONE',  ( 0.000000000000000000, 1.000000000000000000, 1.224646799147350002E-16 ) ) ;
#12377 = EDGE_CURVE ( 'NONE', #9431, #14723, #1321, .T. ) ;
#12378 = CARTESIAN_POINT ( 'NONE',  ( -15.39025577592761174, -21.58198560776530783, 57.00231026484399166 ) ) ;
#12379 = VECTOR ( 'NONE', #13549, 1000.000000000000000 ) ;
#12380 = DIRECTION ( 'NONE',  ( 1.000000000000000000, 1.201369187114119994E-15, 9.616040805000176517E-16 ) ) ;
#12381 = DIRECTION ( 'NONE',  ( 0.9757243316563982694, 0.01146169732403566101, 0.2187022133132789925 ) ) ;
#12382 = ORIENTED_EDGE ( 'NONE', *, *, #8697, .F. ) ;
#12383 = DIRECTION ( 'NONE',  ( -1.000000000000000000, 1.291538348938060198E-32, -1.054621095516909827E-16 ) ) ;
#12384 = CARTESIAN_POINT ( 'NONE',  ( -7.640804079088249878, -45.98079939124116322, -3.051398076617611643 ) ) ;
#12385 = AXIS2_PLACEMENT_3D ( 'NONE', #12813, #10273, #14939 ) ;
#12386 = VERTEX_POINT ( 'NONE', #2665 ) ;
#12388 = ORIENTED_EDGE ( 'NONE', *, *, #5588, .F. ) ;
#12387 = CARTESIAN_POINT ( 'NONE',  ( -18.86735971344653962, -5.080035572537331845, 56.85231026484398598 ) ) ;
#12389 = ORIENTED_EDGE ( 'NONE', *, *, #5260, .T. ) ;
#12390 = DIRECTION ( 'NONE',  ( -8.018662683283438208E-16, 5.975035461963189015E-16, 1.000000000000000000 ) ) ;
#12391 = VECTOR ( 'NONE', #5556, 1000.000000000000114 ) ;
#12392 = CARTESIAN_POINT ( 'NONE',  ( -7.769540243250969702, -46.58425354491494375, 56.19700617964608114 ) ) ;
#12393 = DIRECTION ( 'NONE',  ( 0.5975035461963188466, 0.8018662683283437342, 0.000000000000000000 ) ) ;
#12394 = CIRCLE ( 'NONE', #3605, 9.974999999999999645 ) ;
#12395 = PRODUCT_DEFINITION_SHAPE ( 'NONE', 'NONE',  #15128 ) ;
#12396 = EDGE_CURVE ( 'NONE', #1944, #280, #14294, .T. ) ;
#12397 = CARTESIAN_POINT ( 'NONE',  ( -6.394347403426568377, -9.362396602573261006, 60.59006687612484399 ) ) ;
#12398 = CARTESIAN_POINT ( 'NONE',  ( -17.88573767796789582, -14.53539822139104842, 51.00231026484399166 ) ) ;
#12399 = AXIS2_PLACEMENT_3D ( 'NONE', #1598, #312, #7174 ) ;
#12400 = DIRECTION ( 'NONE',  ( 0.5975035461963189576, 0.8018662683283437342, 0.000000000000000000 ) ) ;
#12401 = CARTESIAN_POINT ( 'NONE',  ( -15.84999713957374645, -16.49322540957318495, 57.00231026484398456 ) ) ;
#12402 = CIRCLE ( 'NONE', #2876, 0.4500000000000011768 ) ;
#12403 = ORIENTED_EDGE ( 'NONE', *, *, #9064, .F. ) ;
#12404 = CARTESIAN_POINT ( 'NONE',  ( 14.68618260102870288, -27.24056927272615880, 46.46206422150100224 ) ) ;
#12405 = EDGE_LOOP ( 'NONE', ( #9194, #11711, #1026, #7912 ) ) ;
#12407 = ORIENTED_EDGE ( 'NONE', *, *, #13372, .T. ) ;
#12406 = CARTESIAN_POINT ( 'NONE',  ( -7.425287632467987287, -13.60480674405941492, 57.00231026484399166 ) ) ;
#12408 = EDGE_LOOP ( 'NONE', ( #9527, #536, #12689, #11373 ) ) ;
#12409 =( REPRESENTATION_RELATIONSHIP ('NONE','NONE', #2372, #13495 ) REPRESENTATION_RELATIONSHIP_WITH_TRANSFORMATION ( #12762 )SHAPE_REPRESENTATION_RELATIONSHIP( ) );
#12410 = CARTESIAN_POINT ( 'NONE',  ( -34.99969986081099904, -20.37340439622244048, 51.53354502093799994 ) ) ;
#12412 = ORIENTED_EDGE ( 'NONE', *, *, #4384, .F. ) ;
#12411 = DIRECTION ( 'NONE',  ( 1.000000000000000000, 1.201369187114119994E-15, 9.616040805000176517E-16 ) ) ;
#12413 = DIRECTION ( 'NONE',  ( 0.000000000000000000, -1.000000000000000000, -1.224646799147350002E-16 ) ) ;
#12414 = AXIS2_PLACEMENT_3D ( 'NONE', #1867, #1637, #3010 ) ;
#12415 = EDGE_CURVE ( 'NONE', #2536, #4202, #12930, .T. ) ;
#12416 = VECTOR ( 'NONE', #14066, 999.9999999999998863 ) ;
#12417 = CARTESIAN_POINT ( 'NONE',  ( -5.499699860810998153, -46.50737899243799944, -5.497689735156003010 ) ) ;
#12418 = AXIS2_PLACEMENT_3D ( 'NONE', #5207, #12102, #7573 ) ;
#12419 = DIRECTION ( 'NONE',  ( 0.000000000000000000, 0.000000000000000000, 1.000000000000000000 ) ) ;
#12420 = EDGE_CURVE ( 'NONE', #413, #9544, #8379, .T. ) ;
#12421 = CARTESIAN_POINT ( 'NONE',  ( -16.17213342976032209, -5.460076146431361188, 56.85231026484398598 ) ) ;
#12422 = DIRECTION ( 'NONE',  ( -0.8018662683283437342, 0.5975035461963188466, -1.000000000000000078E-15 ) ) ;
#12423 = EDGE_LOOP ( 'NONE', ( #527, #9502, #11879, #4697 ) ) ;
#12424 = CARTESIAN_POINT ( 'NONE',  ( 18.35357463111971654, -25.46302391628681505, 40.34329577599203276 ) ) ;
#12425 = EDGE_LOOP ( 'NONE', ( #1532, #4866, #4394, #10257 ) ) ;
#12426 = CARTESIAN_POINT ( 'NONE',  ( -22.61924992783766797, -9.696439889920343447, 56.85231026484398598 ) ) ;
#12427 = VERTEX_POINT ( 'NONE', #13157 ) ;
#12428 = ORIENTED_EDGE ( 'NONE', *, *, #13750, .T. ) ;
#12429 = CARTESIAN_POINT ( 'NONE',  ( -24.41321522311770664, -15.21339595774672127, 57.00231026484397745 ) ) ;
#12430 = VERTEX_POINT ( 'NONE', #5941 ) ;
#12431 = DIRECTION ( 'NONE',  ( 1.000000000000000000, 1.201369187114119994E-15, 9.616040805000176517E-16 ) ) ;
#12432 = EDGE_CURVE ( 'NONE', #7870, #5530, #6828, .T. ) ;
#12433 = DIRECTION ( 'NONE',  ( 1.000000000000000000, 0.000000000000000000, 0.000000000000000000 ) ) ;
#12434 = LINE ( 'NONE', #12288, #8773 ) ;
#12435 = EDGE_CURVE ( 'NONE', #15030, #14193, #1363, .T. ) ;
#12436 = LINE ( 'NONE', #3096, #8982 ) ;
#12437 = ADVANCED_FACE ( 'NONE', ( #4875 ), #4657, .F. ) ;
#12438 = CARTESIAN_POINT ( 'NONE',  ( 9.000300139189000959, -32.00737899243799944, -4.178074911655800250 ) ) ;
#12440 = CARTESIAN_POINT ( 'NONE',  ( 4.917000788749030349, 5.971976172174768394, 29.53007407726659750 ) ) ;
#12439 = DIRECTION ( 'NONE',  ( -1.000000000000000000, 1.291538348938060198E-32, -1.054621095516909827E-16 ) ) ;
#12441 = ORIENTED_EDGE ( 'NONE', *, *, #6004, .T. ) ;
#12442 = CARTESIAN_POINT ( 'NONE',  ( -9.002116193859002635, -10.70790913352571927, 56.85231026484400019 ) ) ;
#12443 = VECTOR ( 'NONE', #2698, 999.9999999999998863 ) ;
#12444 = CARTESIAN_POINT ( 'NONE',  ( -8.430459378593662123, -7.816413432484393020, 56.85231026484400019 ) ) ;
#12445 = ORIENTED_EDGE ( 'NONE', *, *, #14784, .F. ) ;
#12446 = ADVANCED_FACE ( 'NONE', ( #14142 ), #10619, .T. ) ;
#12447 = CARTESIAN_POINT ( 'NONE',  ( -15.49969986081092088, -13.50737899243822504, 57.00231026484397745 ) ) ;
#12448 = LINE ( 'NONE', #9790, #7377 ) ;
#12449 = DIRECTION ( 'NONE',  ( -8.018662683283438208E-16, 5.975035461963189015E-16, 1.000000000000000000 ) ) ;
#12450 = FACE_OUTER_BOUND ( 'NONE', #14586, .T. ) ;
#12451 = ORIENTED_EDGE ( 'NONE', *, *, #4682, .T. ) ;
#12452 = CARTESIAN_POINT ( 'NONE',  ( -15.34686821047329808, -23.48120812104550481, 54.00231026484399166 ) ) ;
#12453 = CIRCLE ( 'NONE', #13405, 1.599999999999999201 ) ;
#12454 = CARTESIAN_POINT ( 'NONE',  ( -22.86200450971638531, -18.81376385001357932, 56.85231026484398598 ) ) ;
#12455 = EDGE_CURVE ( 'NONE', #7227, #4677, #5225, .T. ) ;
#12456 = EDGE_CURVE ( 'NONE', #6725, #15087, #13001, .T. ) ;
#12457 = VECTOR ( 'NONE', #14818, 1000.000000000000114 ) ;
#12458 = CARTESIAN_POINT ( 'NONE',  ( 16.50882759085403606, -72.74114253180582068, 53.29094142560926173 ) ) ;
#12459 = FACE_OUTER_BOUND ( 'NONE', #8126, .T. ) ;
#12460 = CYLINDRICAL_SURFACE ( 'NONE', #6726, 3.249999999999999556 ) ;
#12461 = FACE_OUTER_BOUND ( 'NONE', #11759, .T. ) ;
#12462 = ORIENTED_EDGE ( 'NONE', *, *, #3733, .F. ) ;
#12463 = LINE ( 'NONE', #4048, #4585 ) ;
#12464 = CARTESIAN_POINT ( 'NONE',  ( -23.49969986081102036, -49.19367049345326848, -10.18398123617125428 ) ) ;
#12465 = VERTEX_POINT ( 'NONE', #9545 ) ;
#12467 = ORIENTED_EDGE ( 'NONE', *, *, #1503, .T. ) ;
#12466 = CARTESIAN_POINT ( 'NONE',  ( -7.016473591028808521, -8.259951331604913349, 57.00231026484399166 ) ) ;
#12468 = ORIENTED_EDGE ( 'NONE', *, *, #102, .F. ) ;
#12469 = EDGE_CURVE ( 'NONE', #2788, #4722, #11930, .T. ) ;
#12470 = LINE ( 'NONE', #7706, #5186 ) ;
#12471 = DIRECTION ( 'NONE',  ( 0.7350174335289111349, -0.6780482080269607525, 9.945218953682729003E-16 ) ) ;
#12472 = VECTOR ( 'NONE', #14709, 1000.000000000000114 ) ;
#12473 = LINE ( 'NONE', #6482, #14715 ) ;
#12474 = LINE ( 'NONE', #995, #4027 ) ;
#12475 = B_SPLINE_CURVE_WITH_KNOTS ( 'NONE', 3,
 ( #6503, #4073, #10028, #13490, #11113, #12265, #5296, #5147, #634, #6433, #10967, #4153, #2930, #7658, #4001, #8660, #8886, #1857 ),
 .UNSPECIFIED., .F., .F.,
 ( 4, 2, 2, 2, 2, 2, 2, 2, 4 ),
 ( 0.007091598226763312293, 0.007978859691346384259, 0.008866121155929454489, 0.009753382620512526455, 0.01064064408509559842, 0.01152790554967867039, 0.01241516701426174235, 0.01330242847884481258, 0.01418968994342788455 ),
 .UNSPECIFIED. ) ;
#12476 = CARTESIAN_POINT ( 'NONE',  ( -12.51218212982932165, -9.498047650796509700, 51.00231026484399166 ) ) ;
#12477 = CARTESIAN_POINT ( 'NONE',  ( -17.20133171717847631, -6.639650181150215325, 56.85231026484398598 ) ) ;
#12478 = LINE ( 'NONE', #14692, #5480 ) ;
#12479 = CARTESIAN_POINT ( 'NONE',  ( -13.96026682931439211, -23.36287344688023992, 56.85231026484400019 ) ) ;
#12480 = VERTEX_POINT ( 'NONE', #1442 ) ;
#12481 = CARTESIAN_POINT ( 'NONE',  ( 17.85288399792872127, -29.68312937030077236, 41.35546770520703319 ) ) ;
#12482 = ORIENTED_EDGE ( 'NONE', *, *, #1754, .F. ) ;
#12483 = CARTESIAN_POINT ( 'NONE',  ( -24.55043086433169819, -12.83990741858047357, 57.00231026484397745 ) ) ;
#12485 = ORIENTED_EDGE ( 'NONE', *, *, #11411, .T. ) ;
#12484 = CARTESIAN_POINT ( 'NONE',  ( -7.541197117963764462, -45.30952225410057110, -7.694240868337988815 ) ) ;
#12486 = VERTEX_POINT ( 'NONE', #3581 ) ;
#12487 = EDGE_CURVE ( 'NONE', #5474, #4089, #12303, .T. ) ;
#12488 = DIRECTION ( 'NONE',  ( -8.018662683283438208E-16, 5.975035461963189015E-16, 1.000000000000000000 ) ) ;
#12489 = ORIENTED_EDGE ( 'NONE', *, *, #10616, .T. ) ;
#12490 = FACE_OUTER_BOUND ( 'NONE', #12077, .T. ) ;
#12491 = DIRECTION ( 'NONE',  ( 0.5975035461963187355, 0.8018662683283439563, 0.000000000000000000 ) ) ;
#12492 = CARTESIAN_POINT ( 'NONE',  ( -10.16926643994361967, -19.57302854922115287, 56.85231026484400019 ) ) ;
#12493 = CARTESIAN_POINT ( 'NONE',  ( -30.62513859619093637, -27.95036676736707548, -14.90232471354688037 ) ) ;
#12494 = ORIENTED_EDGE ( 'NONE', *, *, #13441, .F. ) ;
#12495 = CARTESIAN_POINT ( 'NONE',  ( 17.02925260421022813, -23.75019164044109132, 42.87573938909707039 ) ) ;
#12496 = ORIENTED_EDGE ( 'NONE', *, *, #4578, .F. ) ;
#12497 = DIRECTION ( 'NONE',  ( 0.000000000000000000, 1.700257036304450134E-17, -1.000000000000000000 ) ) ;
#12498 = VERTEX_POINT ( 'NONE', #10776 ) ;
#12499 = ORIENTED_EDGE ( 'NONE', *, *, #8697, .T. ) ;
#12500 = EDGE_CURVE ( 'NONE', #3416, #2925, #298, .T. ) ;
#12501 = FACE_OUTER_BOUND ( 'NONE', #3393, .T. ) ;
#12502 = ORIENTED_EDGE ( 'NONE', *, *, #7374, .T. ) ;
#12503 = DIRECTION ( 'NONE',  ( -0.9997391571607664451, -0.02283895005205794498, -7.880107536067222722E-16 ) ) ;
#12504 = FACE_BOUND ( 'NONE', #3505, .T. ) ;
#12505 = VECTOR ( 'NONE', #5458, 1000.000000000000227 ) ;
#12506 = CARTESIAN_POINT ( 'NONE',  ( -10.22659806069228416, -90.55000404333293318, -6.537620383987239769 ) ) ;
#12507 = VECTOR ( 'NONE', #9189, 1000.000000000000227 ) ;
#12508 = PLANE ( 'NONE',  #1424 ) ;
#12509 = CARTESIAN_POINT ( 'NONE',  ( -20.18599136182623965, -36.50737899243796392, 27.50231026484402719 ) ) ;
#12511 = CARTESIAN_POINT ( 'NONE',  ( 4.926418148162898802, 5.967462257416214833, 29.52493280993808966 ) ) ;
#12510 = CARTESIAN_POINT ( 'NONE',  ( -10.12827371166237533, -110.0073789924380065, -5.497689735155995017 ) ) ;
#12512 = ORIENTED_EDGE ( 'NONE', *, *, #12962, .F. ) ;
#12513 = DIRECTION ( 'NONE',  ( 0.000000000000000000, -1.000000000000000000, -1.224646799147350002E-16 ) ) ;
#12514 = FACE_OUTER_BOUND ( 'NONE', #11912, .T. ) ;
#12515 = VERTEX_POINT ( 'NONE', #8693 ) ;
#12516 = ORIENTED_EDGE ( 'NONE', *, *, #13986, .T. ) ;
#12517 = CARTESIAN_POINT ( 'NONE',  ( -14.76203582817000104, -107.1622034095870077, -6.087689735155999315 ) ) ;
#12518 = EDGE_CURVE ( 'NONE', #626, #8256, #6389, .T. ) ;
#12519 = VECTOR ( 'NONE', #11071, 999.9999999999998863 ) ;
#12520 = CYLINDRICAL_SURFACE ( 'NONE', #2500, 1.074999999999999512 ) ;
#12521 = VECTOR ( 'NONE', #2832, 1000.000000000000114 ) ;
#12522 = CYLINDRICAL_SURFACE ( 'NONE', #11822, 10.00000000000000000 ) ;
#12523 = ORIENTED_EDGE ( 'NONE', *, *, #14266, .T. ) ;
#12524 = CARTESIAN_POINT ( 'NONE',  ( -15.49969986081099727, -105.7207835729139305, -8.916635449454062723 ) ) ;
#12525 = CIRCLE ( 'NONE', #8107, 1.750000000000000666 ) ;
#12526 = AXIS2_PLACEMENT_3D ( 'NONE', #9240, #1135, #13920 ) ;
#12527 = EDGE_CURVE ( 'NONE', #3602, #11369, #13299, .T. ) ;
#12528 = DIRECTION ( 'NONE',  ( 0.6061090314442014737, -0.7953815700667020705, 9.612616959383187437E-16 ) ) ;
#12529 = EDGE_CURVE ( 'NONE', #14910, #951, #382, .T. ) ;
#12530 = PRODUCT_CONTEXT ( 'NONE', #9478, 'mechanical' ) ;
#12531 = CARTESIAN_POINT ( 'NONE',  ( -7.886584594865169606, -46.96511696614940234, 21.96004823855531640 ) ) ;
#12532 = VECTOR ( 'NONE', #11965, 1000.000000000000000 ) ;
#12533 = VECTOR ( 'NONE', #10093, 1000.000000000000114 ) ;
#12534 = FACE_OUTER_BOUND ( 'NONE', #11726, .T. ) ;
#12535 = DIRECTION ( 'NONE',  ( 3.839882694219489529E-17, -1.000000000000000000, 0.000000000000000000 ) ) ;
#12536 = VERTEX_POINT ( 'NONE', #664 ) ;
#12537 = CARTESIAN_POINT ( 'NONE',  ( -10.49759577181166215, -90.58864147777146059, -3.450279645307360976 ) ) ;
#12538 = ADVANCED_FACE ( 'NONE', ( #1663 ), #6463, .F. ) ;
#12539 = CARTESIAN_POINT ( 'NONE',  ( -7.527660810972179206, -45.17397571328393013, -3.380064858389232985 ) ) ;
#12540 = CARTESIAN_POINT ( 'NONE',  ( -21.89842656004739396, -7.071732433740530510, 56.85231026484398598 ) ) ;
#12541 = ADVANCED_FACE ( 'NONE', ( #6316 ), #1588, .T. ) ;
#12542 = EDGE_CURVE ( 'NONE', #4535, #6874, #5701, .T. ) ;
#12543 = ORIENTED_EDGE ( 'NONE', *, *, #2920, .F. ) ;
#12545 = ORIENTED_EDGE ( 'NONE', *, *, #847, .F. ) ;
#12544 = CARTESIAN_POINT ( 'NONE',  ( -7.663319311905077313, -46.12821245145848792, 46.98080104517658384 ) ) ;
#12546 = ORIENTED_EDGE ( 'NONE', *, *, #5133, .T. ) ;
#12547 = B_SPLINE_CURVE_WITH_KNOTS ( 'NONE', 3,
 ( #813, #10129, #8366, #14112 ),
 .UNSPECIFIED., .F., .F.,
 ( 4, 4 ),
 ( 0.01169941957287879905, 0.01381006638855979997 ),
 .UNSPECIFIED. ) ;
#12548 = CARTESIAN_POINT ( 'NONE',  ( 1.872105016583406778, -24.05954647699557114, -13.82452877272129399 ) ) ;
#12549 = CARTESIAN_POINT ( 'NONE',  ( -7.550611734114103690, -45.55128411564821533, 56.15027137728581863 ) ) ;
#12550 = AXIS2_PLACEMENT_3D ( 'NONE', #3409, #8059, #11662 ) ;
#12551 = AXIS2_PLACEMENT_3D ( 'NONE', #3595, #8176, #4978 ) ;
#12553 = VECTOR ( 'NONE', #12922, 999.9999999999998863 ) ;
#12552 = PLANE ( 'NONE',  #5668 ) ;
#12554 = CARTESIAN_POINT ( 'NONE',  ( -8.185397854257590922, -47.75120526332403159, 42.32787638714851397 ) ) ;
#12555 = CARTESIAN_POINT ( 'NONE',  ( -8.200120392665880331, -6.662954729433940848, 60.99550424616020194 ) ) ;
#12556 = DIRECTION ( 'NONE',  ( -0.9085715390340278752, 0.4177292884839868825, -9.781476007338035090E-16 ) ) ;
#12557 = VECTOR ( 'NONE', #12000, 1000.000000000000000 ) ;
#12558 = DIRECTION ( 'NONE',  ( 0.9183863840214729901, 0.3956847857120157075, 4.999999999999999402E-16 ) ) ;
#12559 = ORIENTED_EDGE ( 'NONE', *, *, #8424, .T. ) ;
#12560 = LINE ( 'NONE', #4525, #7607 ) ;
#12561 = EDGE_CURVE ( 'NONE', #1793, #13470, #7395, .T. ) ;
#12562 = ORIENTED_EDGE ( 'NONE', *, *, #7865, .T. ) ;
#12563 = CARTESIAN_POINT ( 'NONE',  ( -7.499699860810999041, -44.50737899243799944, -109.5506571639849938 ) ) ;
#12565 = ORIENTED_EDGE ( 'NONE', *, *, #918, .T. ) ;
#12564 = CARTESIAN_POINT ( 'NONE',  ( -25.16886795621463691, -10.89431112827525361, 60.44430563842290383 ) ) ;
#12566 = VERTEX_POINT ( 'NONE', #3033 ) ;
#12567 = EDGE_CURVE ( 'NONE', #9329, #2702, #4517, .T. ) ;
#12568 = CARTESIAN_POINT ( 'NONE',  ( -32.87150473820536689, -24.05954647699559601, 52.82914930240931994 ) ) ;
#12569 = VERTEX_POINT ( 'NONE', #14440 ) ;
#12570 = AXIS2_PLACEMENT_3D ( 'NONE', #3857, #13207, #8739 ) ;
#12571 = CARTESIAN_POINT ( 'NONE',  ( -15.49969986081099904, -27.00737899243800300, -13.49768973515600301 ) ) ;
#12572 = AXIS2_PLACEMENT_3D ( 'NONE', #1161, #461, #8702 ) ;
#12573 = CYLINDRICAL_SURFACE ( 'NONE', #12231, 3.000000000000000000 ) ;
#12574 = EDGE_CURVE ( 'NONE', #12480, #9659, #14519, .T. ) ;
#12575 = ORIENTED_EDGE ( 'NONE', *, *, #13109, .F. ) ;
#12576 = DIRECTION ( 'NONE',  ( 8.018662683283438208E-16, -5.975035461963189015E-16, -1.000000000000000000 ) ) ;
#12577 = CIRCLE ( 'NONE', #4022, 0.1500000000000015488 ) ;
#12578 = CARTESIAN_POINT ( 'NONE',  ( -8.131654986474892155, -16.81240013151894530, 56.85231026484400019 ) ) ;
#12579 = ORIENTED_EDGE ( 'NONE', *, *, #4551, .T. ) ;
#12580 = CARTESIAN_POINT ( 'NONE',  ( 15.03590892877081409, -25.29102231028643644, 45.98015512529381965 ) ) ;
#12581 = ORIENTED_EDGE ( 'NONE', *, *, #7673, .T. ) ;
#12582 = DIRECTION ( 'NONE',  ( 0.000000000000000000, 0.000000000000000000, -1.000000000000000000 ) ) ;
#12583 = EDGE_LOOP ( 'NONE', ( #8903, #10062, #5831, #8859 ) ) ;
#12584 = EDGE_LOOP ( 'NONE', ( #6706, #2758, #4558, #817 ) ) ;
#12585 = PRESENTATION_LAYER_ASSIGNMENT (  '', '', ( #1096 ) ) ;
#12586 = PLANE ( 'NONE',  #10045 ) ;
#12587 = VERTEX_POINT ( 'NONE', #1892 ) ;
#12588 = LINE ( 'NONE', #2101, #13996 ) ;
#12589 = DIRECTION ( 'NONE',  ( 0.1960948578651655061, -0.9805849309054471830, 7.431448254773943634E-16 ) ) ;
#12590 = CARTESIAN_POINT ( 'NONE',  ( -10.59040657616195524, -90.60431240515791274, -7.677386969860795496 ) ) ;
#12591 = AXIS2_PLACEMENT_3D ( 'NONE', #22, #10414, #1235 ) ;
#12592 = ADVANCED_FACE ( 'NONE', ( #7469 ), #595, .F. ) ;
#12593 = CARTESIAN_POINT ( 'NONE',  ( -12.51218212982931810, -9.498047650796513253, 45.50231026484398456 ) ) ;
#12594 = DIRECTION ( 'NONE',  ( 1.000000000000000000, 1.201369187114119994E-15, 9.616040805000176517E-16 ) ) ;
#12596 = CARTESIAN_POINT ( 'NONE',  ( 4.527565447144258570, 6.159096188232942914, 29.73988678045787637 ) ) ;
#12595 = LINE ( 'NONE', #5692, #14478 ) ;
#12597 = ORIENTED_EDGE ( 'NONE', *, *, #13048, .F. ) ;
#12598 = DIRECTION ( 'NONE',  ( -0.7276687409742212953, -0.6859287159822015090, -1.736481776669299976E-16 ) ) ;
#12599 = CARTESIAN_POINT ( 'NONE',  ( -19.99969986081099904, -13.50737899243800122, -13.01695671647154917 ) ) ;
#12600 = VERTEX_POINT ( 'NONE', #7543 ) ;
#12601 = EDGE_LOOP ( 'NONE', ( #4018, #7598, #8900, #3770 ) ) ;
#12602 = CARTESIAN_POINT ( 'NONE',  ( -15.86970092169881141, -16.66117552174622318, 57.00231026484397745 ) ) ;
#12603 = DIRECTION ( 'NONE',  ( 1.000000000000000000, 1.000000000000000078E-15, 1.000000000000000078E-15 ) ) ;
#12604 = DIRECTION ( 'NONE',  ( 0.000000000000000000, 0.000000000000000000, -1.000000000000000000 ) ) ;
#12605 = ORIENTED_EDGE ( 'NONE', *, *, #2495, .T. ) ;
#12606 = CARTESIAN_POINT ( 'NONE',  ( -18.09969986081100046, -107.0941666664711676, -4.789471339975055919 ) ) ;
#12607 = CARTESIAN_POINT ( 'NONE',  ( 0.8003001391889992266, 3.992621007561997892, 24.26206422150100295 ) ) ;
#12608 = EDGE_CURVE ( 'NONE', #5496, #4806, #8700, .T. ) ;
#12609 = CARTESIAN_POINT ( 'NONE',  ( 6.045543233663400073, 12.99262100756199878, 16.16206422150100153 ) ) ;
#12610 = LINE ( 'NONE', #3421, #4797 ) ;
#12611 = CARTESIAN_POINT ( 'NONE',  ( -12.52039621090187893, -4.935039769003430443, 56.85231026484398598 ) ) ;
#12612 = EDGE_CURVE ( 'NONE', #10845, #6478, #14588, .T. ) ;
#12613 = AXIS2_PLACEMENT_3D ( 'NONE', #9446, #3637, #8369 ) ;
#12614 = VERTEX_POINT ( 'NONE', #13452 ) ;
#12615 = CARTESIAN_POINT ( 'NONE',  ( -10.19698273680794820, -90.54727021874583670, -4.632518811245576629 ) ) ;
#12616 = CIRCLE ( 'NONE', #6002, 9.974999999999999645 ) ;
#12617 = CARTESIAN_POINT ( 'NONE',  ( -35.90489723645450226, 5.977487861575448314, 29.53635566902382337 ) ) ;
#12618 = DIRECTION ( 'NONE',  ( 0.5975035461963188466, 0.8018662683283437342, 0.000000000000000000 ) ) ;
#12619 = DIRECTION ( 'NONE',  ( 0.5975035461963188466, 0.8018662683283437342, 0.000000000000000000 ) ) ;
#12620 = ORIENTED_EDGE ( 'NONE', *, *, #3346, .T. ) ;
#12621 = DIRECTION ( 'NONE',  ( -3.839882694219489529E-17, 1.000000000000000000, 0.000000000000000000 ) ) ;
#12622 = ORIENTED_EDGE ( 'NONE', *, *, #5335, .T. ) ;
#12623 = CARTESIAN_POINT ( 'NONE',  ( -2.716578225681299141, -32.00737899243799944, -15.75165123257469801 ) ) ;
#12624 = CARTESIAN_POINT ( 'NONE',  ( -10.62325334976782720, -50.85476156143290183, 56.68445949013308649 ) ) ;
#12625 = EDGE_CURVE ( 'NONE', #3870, #1460, #2957, .T. ) ;
#12626 = LINE ( 'NONE', #2142, #9584 ) ;
#12627 = CARTESIAN_POINT ( 'NONE',  ( -8.005579240875389857, -47.31158775777677761, 42.12977053007920603 ) ) ;
#12628 = EDGE_CURVE ( 'NONE', #6762, #11659, #519, .T. ) ;
#12629 = CARTESIAN_POINT ( 'NONE',  ( -6.020613275810588583, -10.26707144315182063, 60.49515945283604879 ) ) ;
#12630 = EDGE_CURVE ( 'NONE', #8099, #12721, #4002, .T. ) ;
#12631 = FACE_OUTER_BOUND ( 'NONE', #13929, .T. ) ;
#12632 = FACE_OUTER_BOUND ( 'NONE', #11598, .T. ) ;
#12633 = CARTESIAN_POINT ( 'NONE',  ( -15.49969986081092088, -13.50737899243822504, 56.85231026484398598 ) ) ;
#12634 = EDGE_LOOP ( 'NONE', ( #12445, #14305, #5236, #5005 ) ) ;
#12635 = DIRECTION ( 'NONE',  ( -8.018662683283438208E-16, 5.975035461963189015E-16, 1.000000000000000000 ) ) ;
#12636 = CIRCLE ( 'NONE', #1136, 2.499999999999998668 ) ;
#12637 = ORIENTED_EDGE ( 'NONE', *, *, #6696, .T. ) ;
#12638 = DIRECTION ( 'NONE',  ( -0.5491495666976170531, 0.8357240892757724637, -9.396926207859082113E-16 ) ) ;
#12640 = EDGE_LOOP ( 'NONE', ( #10006, #2015, #15004, #4459 ) ) ;
#12639 = PLANE ( 'NONE',  #1545 ) ;
#12641 = EDGE_CURVE ( 'NONE', #9932, #2536, #744, .T. ) ;
#12642 = ORIENTED_EDGE ( 'NONE', *, *, #14726, .F. ) ;
#12643 = CARTESIAN_POINT ( 'NONE',  ( -12.95343247850694723, -15.40470757524832912, 57.00231026484399166 ) ) ;
#12644 = ORIENTED_EDGE ( 'NONE', *, *, #181, .T. ) ;
#12645 =( GEOMETRIC_REPRESENTATION_CONTEXT ( 3 ) GLOBAL_UNCERTAINTY_ASSIGNED_CONTEXT ( ( #6597 ) ) GLOBAL_UNIT_ASSIGNED_CONTEXT ( ( #9580, #3772, #12966 ) ) REPRESENTATION_CONTEXT ( 'NONE', 'WORKASPACE' ) );
#12646 = CARTESIAN_POINT ( 'NONE',  ( 4.000300139189000959, -20.37340439622242982, -17.99768973515599768 ) ) ;
#12647 = AXIS2_PLACEMENT_3D ( 'NONE', #10688, #10771, #14289 ) ;
#12648 = DIRECTION ( 'NONE',  ( 1.054621095516909827E-16, 1.224646799147350002E-16, -1.000000000000000000 ) ) ;
#12649 = EDGE_CURVE ( 'NONE', #6778, #2175, #7035, .T. ) ;
#12650 = EDGE_CURVE ( 'NONE', #6401, #15001, #3510, .T. ) ;
#12651 = CIRCLE ( 'NONE', #1406, 2.000000000000001776 ) ;
#12652 = CIRCLE ( 'NONE', #4843, 9.974999999999999645 ) ;
#12653 = EDGE_CURVE ( 'NONE', #1455, #13413, #10219, .T. ) ;
#12654 = ORIENTED_EDGE ( 'NONE', *, *, #8050, .T. ) ;
#12655 = LINE ( 'NONE', #5748, #14485 ) ;
#12656 = VERTEX_POINT ( 'NONE', #6761 ) ;
#12657 = CARTESIAN_POINT ( 'NONE',  ( 17.66731393161950336, -24.11684619341258085, 41.71177241952297265 ) ) ;
#12658 = ORIENTED_EDGE ( 'NONE', *, *, #14408, .F. ) ;
#12659 = VERTEX_POINT ( 'NONE', #5704 ) ;
#12660 = EDGE_LOOP ( 'NONE', ( #9393, #13709, #1557, #13629, #7278, #10654, #29, #10443 ) ) ;
#12661 = ORIENTED_EDGE ( 'NONE', *, *, #14125, .T. ) ;
#12662 = VECTOR ( 'NONE', #11045, 1000.000000000000000 ) ;
#12664 = EDGE_CURVE ( 'NONE', #5453, #2941, #3190, .T. ) ;
#12663 = LINE ( 'NONE', #8127, #14484 ) ;
#12665 = AXIS2_PLACEMENT_3D ( 'NONE', #226, #9400, #3890 ) ;
#12666 = CARTESIAN_POINT ( 'NONE',  ( -15.49969986081092088, -13.50737899243822504, 56.85231026484398598 ) ) ;
#12667 = CARTESIAN_POINT ( 'NONE',  ( -15.49969986081099194, -36.50737899243799944, 11.50231026484399699 ) ) ;
#12669 = CARTESIAN_POINT ( 'NONE',  ( 4.795664383891133475, 6.030134292646086358, 29.59621904580064822 ) ) ;
#12668 = CARTESIAN_POINT ( 'NONE',  ( -16.02866194833901403, -110.0647956111179866, -10.55728977053499129 ) ) ;
#12670 = CIRCLE ( 'NONE', #8253, 1.750000000000000666 ) ;
#12671 = ORIENTED_EDGE ( 'NONE', *, *, #5943, .T. ) ;
#12672 = DIRECTION ( 'NONE',  ( 8.018662683283438208E-16, -5.975035461963189015E-16, -1.000000000000000000 ) ) ;
#12673 = PLANE ( 'NONE',  #3268 ) ;
#12674 = EDGE_LOOP ( 'NONE', ( #10146, #12109, #8411, #1421 ) ) ;
#12675 = ORIENTED_EDGE ( 'NONE', *, *, #9986, .T. ) ;
#12676 = FACE_OUTER_BOUND ( 'NONE', #133, .T. ) ;
#12677 = DIRECTION ( 'NONE',  ( 0.000000000000000000, -1.000000000000000000, -1.224646799147350002E-16 ) ) ;
#12678 = DIRECTION ( 'NONE',  ( 0.6859287159822015090, -0.7276687409742212953, 9.848077530122081084E-16 ) ) ;
#12679 = ORIENTED_EDGE ( 'NONE', *, *, #10855, .F. ) ;
#12680 = LINE ( 'NONE', #7990, #1738 ) ;
#12681 = EDGE_CURVE ( 'NONE', #12888, #2185, #7916, .T. ) ;
#12682 = VECTOR ( 'NONE', #12828, 1000.000000000000000 ) ;
#12683 = DIRECTION ( 'NONE',  ( 1.000000000000000000, 1.000000000000000078E-15, 0.000000000000000000 ) ) ;
#12684 = PLANE ( 'NONE',  #10945 ) ;
#12685 = CIRCLE ( 'NONE', #713, 37.50000000000000000 ) ;
#12686 = PRODUCT_DEFINITION_FORMATION_WITH_SPECIFIED_SOURCE ( 'ANY', '', #10923, .NOT_KNOWN. ) ;
#12687 = DIRECTION ( 'NONE',  ( -0.7805252200231699300, 0.6251242923673516749, -9.993908270190957033E-16 ) ) ;
#12688 = CARTESIAN_POINT ( 'NONE',  ( -15.39025577592761174, -21.58198560776530783, 56.85231026484400019 ) ) ;
#12689 = ORIENTED_EDGE ( 'NONE', *, *, #1065, .T. ) ;
#12690 = CARTESIAN_POINT ( 'NONE',  ( -13.28192010678624868, -91.85033406443031367, -0.6052620916867849088 ) ) ;
#12691 = PLANE ( 'NONE',  #13380 ) ;
#12692 = DIRECTION ( 'NONE',  ( 0.8719950447285833572, 0.4895147004624025300, 4.067366430758019417E-16 ) ) ;
#12693 = CARTESIAN_POINT ( 'NONE',  ( -15.49969986081079654, 1010.738102757666070, -1640.067418128998952 ) ) ;
#12694 = ORIENTED_EDGE ( 'NONE', *, *, #10908, .T. ) ;
#12695 = CARTESIAN_POINT ( 'NONE',  ( -15.14940258204810242, -10.52153257530326158, 57.00231026484397745 ) ) ;
#12696 = ORIENTED_EDGE ( 'NONE', *, *, #14406, .T. ) ;
#12697 = ADVANCED_FACE ( 'NONE', ( #4417 ), #12522, .F. ) ;
#12698 = DIRECTION ( 'NONE',  ( 1.000000000000000000, 1.000000000000000078E-15, 0.000000000000000000 ) ) ;
#12699 = LINE ( 'NONE', #13616, #7759 ) ;
#12700 = CIRCLE ( 'NONE', #1457, 23.00000000000000000 ) ;
#12701 = VECTOR ( 'NONE', #11603, 1000.000000000000000 ) ;
#12702 = EDGE_CURVE ( 'NONE', #6219, #1569, #11224, .T. ) ;
#12703 = CARTESIAN_POINT ( 'NONE',  ( -3.508527451665000463, -45.64135358865355840, -3.997689735156000790 ) ) ;
#12704 = LINE ( 'NONE', #9241, #8420 ) ;
#12705 = B_SPLINE_CURVE_WITH_KNOTS ( 'NONE', 3,
 ( #13406, #5284, #5137, #6275, #483, #9801, #6568, #1693, #7575, #11177, #3990, #13554, #3915, #14619, #2918, #623, #3059, #697 ),
 .UNSPECIFIED., .F., .F.,
 ( 4, 2, 2, 2, 2, 2, 2, 2, 4 ),
 ( 0.002328648564201944281, 0.002729030124645695152, 0.003129411685089445588, 0.003529793245533196459, 0.003930174805976947329, 0.004330556366420697766, 0.004730937926864449070, 0.005131319487308199506, 0.005531701047751949943 ),
 .UNSPECIFIED. ) ;
#12706 = CARTESIAN_POINT ( 'NONE',  ( 9.000300139189000959, -27.00737899243800300, 2.712064221501000461 ) ) ;
#12707 = DIRECTION ( 'NONE',  ( 3.202566417187950042E-16, 1.224646799147350002E-16, -1.000000000000000000 ) ) ;
#12708 = CARTESIAN_POINT ( 'NONE',  ( -35.49969986081099904, -19.50737899243800300, 55.93350807262480373 ) ) ;
#12709 = VECTOR ( 'NONE', #9200, 1000.000000000000114 ) ;
#12710 = DIRECTION ( 'NONE',  ( 0.5975035461963189576, 0.8018662683283437342, 0.000000000000000000 ) ) ;
#12711 = EDGE_LOOP ( 'NONE', ( #13740, #1078, #13703, #9360 ) ) ;
#12712 = CARTESIAN_POINT ( 'NONE',  ( -22.70654572567255158, -20.40389968624656802, 54.00231026484399166 ) ) ;
#12713 = ORIENTED_EDGE ( 'NONE', *, *, #1488, .F. ) ;
#12715 = ORIENTED_EDGE ( 'NONE', *, *, #6382, .F. ) ;
#12714 = CARTESIAN_POINT ( 'NONE',  ( -21.49969986081095996, -67.00737899243799234, -5.497689735156007451 ) ) ;
#12716 = ORIENTED_EDGE ( 'NONE', *, *, #4755, .F. ) ;
#12717 = EDGE_CURVE ( 'NONE', #8073, #7447, #6689, .T. ) ;
#12718 = AXIS2_PLACEMENT_3D ( 'NONE', #39, #8206, #3551 ) ;
#12719 = CARTESIAN_POINT ( 'NONE',  ( -18.09969986081100046, -109.6217528783177784, -2.009566970250350693 ) ) ;
#12720 = EDGE_CURVE ( 'NONE', #364, #5054, #7176, .T. ) ;
#12721 = VERTEX_POINT ( 'NONE', #10294 ) ;
#12722 = DIRECTION ( 'NONE',  ( -1.000000000000000000, 0.000000000000000000, 0.000000000000000000 ) ) ;
#12723 = ADVANCED_FACE ( 'NONE', ( #12450 ), #13821, .T. ) ;
#12724 = LINE ( 'NONE', #8889, #9403 ) ;
#12725 = CARTESIAN_POINT ( 'NONE',  ( -12.11547932532413263, -20.83938426843124603, 56.85231026484400019 ) ) ;
#12726 = EDGE_CURVE ( 'NONE', #15030, #2398, #7988, .T. ) ;
#12727 = VECTOR ( 'NONE', #9571, 1000.000000000000000 ) ;
#12728 = ORIENTED_EDGE ( 'NONE', *, *, #13939, .F. ) ;
#12729 = CARTESIAN_POINT ( 'NONE',  ( -6.938526287600617515, -8.388108336439909607, 56.85231026484400019 ) ) ;
#12730 = EDGE_LOOP ( 'NONE', ( #5077, #13113, #13871, #14928 ) ) ;
#12731 = LINE ( 'NONE', #10190, #3860 ) ;
#12732 = ORIENTED_EDGE ( 'NONE', *, *, #4124, .F. ) ;
#12733 = DIRECTION ( 'NONE',  ( 1.000000000000000000, -1.291538348938060198E-32, 1.054621095516909827E-16 ) ) ;
#12734 = ORIENTED_EDGE ( 'NONE', *, *, #372, .T. ) ;
#12735 = EDGE_LOOP ( 'NONE', ( #4148, #12642, #14938, #5513 ) ) ;
#12736 = ADVANCED_FACE ( 'NONE', ( #2195 ), #6841, .F. ) ;
#12737 = DIRECTION ( 'NONE',  ( 0.000000000000000000, -0.05233595624294329340, -0.9986295347545738332 ) ) ;
#12738 = EDGE_CURVE ( 'NONE', #12036, #1378, #1968, .T. ) ;
#12739 = ORIENTED_EDGE ( 'NONE', *, *, #3176, .F. ) ;
#12740 = DIRECTION ( 'NONE',  ( -8.018662683283438208E-16, 5.975035461963189015E-16, 1.000000000000000000 ) ) ;
#12741 = DIRECTION ( 'NONE',  ( -8.018662683283439195E-16, 5.975035461963190001E-16, 1.000000000000000000 ) ) ;
#12742 = DIRECTION ( 'NONE',  ( 0.000000000000000000, 1.000000000000000000, 1.224646799147350002E-16 ) ) ;
#12743 = VECTOR ( 'NONE', #10063, 1000.000000000000000 ) ;
#12744 = EDGE_CURVE ( 'NONE', #12430, #11072, #5572, .T. ) ;
#12745 = CARTESIAN_POINT ( 'NONE',  ( -16.24959055444668365, -20.54292544936667042, 57.00231026484399166 ) ) ;
#12747 = CARTESIAN_POINT ( 'NONE',  ( 2.500300139188999182, -37.00737899243799944, 19.50231026484398811 ) ) ;
#12746 = DIRECTION ( 'NONE',  ( 0.7737441449604661736, 0.6334982226805353500, 2.419218955996689845E-16 ) ) ;
#12748 = ORIENTED_EDGE ( 'NONE', *, *, #13468, .T. ) ;
#12749 = CARTESIAN_POINT ( 'NONE',  ( -7.517356049973301424, -45.05918421631233173, 42.45528228030804030 ) ) ;
#12750 = CARTESIAN_POINT ( 'NONE',  ( -22.94870171817393256, -18.69135635822624053, 57.00231026484397745 ) ) ;
#12751 = ORIENTED_EDGE ( 'NONE', *, *, #1737, .F. ) ;
#12752 = ORIENTED_EDGE ( 'NONE', *, *, #14236, .F. ) ;
#12753 = CARTESIAN_POINT ( 'NONE',  ( -15.49969986081099904, 22.99262100756200056, 24.21206422150100224 ) ) ;
#12754 = CARTESIAN_POINT ( 'NONE',  ( -15.49969986081099371, -36.50737899243799944, -17.99768973515599768 ) ) ;
#12755 = DIRECTION ( 'NONE',  ( 0.000000000000000000, 0.000000000000000000, 1.000000000000000000 ) ) ;
#12756 = ORIENTED_EDGE ( 'NONE', *, *, #684, .T. ) ;
#12757 = CARTESIAN_POINT ( 'NONE',  ( -21.48581293389291247, -5.528213918555015205, 56.85231026484398598 ) ) ;
#12758 = CIRCLE ( 'NONE', #14363, 0.4500000000000011768 ) ;
#12759 = EDGE_CURVE ( 'NONE', #5586, #3528, #824, .T. ) ;
#12760 = AXIS2_PLACEMENT_3D ( 'NONE', #15070, #4829, #9251 ) ;
#12761 = FACE_OUTER_BOUND ( 'NONE', #9828, .T. ) ;
#12762 = ITEM_DEFINED_TRANSFORMATION ( 'NONE', 'NONE', #15120,  #6789 ) ;
#12763 = CARTESIAN_POINT ( 'NONE',  ( -9.969334273478565933, -7.622966832294271633, 56.85231026484398598 ) ) ;
#12764 = MANIFOLD_SOLID_BREP ( 'Stock-MAS-672-1', #8519 ) ;
#12765 = ADVANCED_FACE ( 'NONE', ( #3644 ), #9528, .F. ) ;
#12766 = EDGE_CURVE ( 'NONE', #1165, #13612, #14050, .T. ) ;
#12767 = DIRECTION ( 'NONE',  ( -1.000000000000000000, -1.201369187114119994E-15, -9.616040805000176517E-16 ) ) ;
#12768 = DIRECTION ( 'NONE',  ( 0.000000000000000000, 1.000000000000000000, 1.224646799147350002E-16 ) ) ;
#12769 = VECTOR ( 'NONE', #9739, 1000.000000000000000 ) ;
#12770 = VERTEX_POINT ( 'NONE', #4946 ) ;
#12771 = CARTESIAN_POINT ( 'NONE',  ( -10.22863128988245229, -90.55140526738702533, -4.451800774622809875 ) ) ;
#12772 = VECTOR ( 'NONE', #7416, 1000.000000000000114 ) ;
#12773 = CARTESIAN_POINT ( 'NONE',  ( -35.31162891843938922, 6.261951257131300963, 29.84176477860722443 ) ) ;
#12774 = DIRECTION ( 'NONE',  ( -8.018662683283439195E-16, 5.975035461963190001E-16, 1.000000000000000000 ) ) ;
#12775 = AXIS2_PLACEMENT_3D ( 'NONE', #3166, #876, #5457 ) ;
#12776 = AXIS2_PLACEMENT_3D ( 'NONE', #4134, #919, #10319 ) ;
#12777 = DIRECTION ( 'NONE',  ( -8.018662683283438208E-16, 5.975035461963189015E-16, 1.000000000000000000 ) ) ;
#12778 = ORIENTED_EDGE ( 'NONE', *, *, #11769, .T. ) ;
#12779 = DIRECTION ( 'NONE',  ( 0.000000000000000000, -9.251858538542971581E-17, 1.000000000000000000 ) ) ;
#12780 = VERTEX_POINT ( 'NONE', #7220 ) ;
#12781 = DIRECTION ( 'NONE',  ( -8.018662683283439195E-16, 5.975035461963190001E-16, 1.000000000000000000 ) ) ;
#12782 = CARTESIAN_POINT ( 'NONE',  ( -11.71495923925436955, -5.812446346369147143, 56.85231026484398598 ) ) ;
#12783 = CARTESIAN_POINT ( 'NONE',  ( -5.499699860811000818, -46.50737899243799944, 16.50231026484399877 ) ) ;
#12784 = DIRECTION ( 'NONE',  ( 0.9957106782009863544, 0.09252159378508258147, 7.431448254773871651E-16 ) ) ;
#12785 = VECTOR ( 'NONE', #11053, 1000.000000000000114 ) ;
#12786 = AXIS2_PLACEMENT_3D ( 'NONE', #8650, #13336, #2839 ) ;
#12787 = CARTESIAN_POINT ( 'NONE',  ( -5.542205825327698676, -14.57691648049767963, 60.36598623123717999 ) ) ;
#12788 = EDGE_CURVE ( 'NONE', #14718, #12356, #6248, .T. ) ;
#12789 = CARTESIAN_POINT ( 'NONE',  ( -15.49969986081092088, -13.50737899243822504, 56.85231026484398598 ) ) ;
#12790 = CARTESIAN_POINT ( 'NONE',  ( -20.60655739512267104, -107.3584631001859719, -7.162689735156004822 ) ) ;
#12791 = CARTESIAN_POINT ( 'NONE',  ( -6.758527451664997798, -49.50737899243800655, -5.497689735156000346 ) ) ;
#12792 = ORIENTED_EDGE ( 'NONE', *, *, #7076, .F. ) ;
#12793 = CARTESIAN_POINT ( 'NONE',  ( -15.47224238247604511, -13.54916519690201149, 56.85231026484398598 ) ) ;
#12794 = PRODUCT_DEFINITION_CONTEXT ( 'detailed design', #1660, 'design' ) ;
#12795 = VERTEX_POINT ( 'NONE', #1114 ) ;
#12796 = LINE ( 'NONE', #11626, #11888 ) ;
#12798 = ORIENTED_EDGE ( 'NONE', *, *, #6216, .T. ) ;
#12797 = CARTESIAN_POINT ( 'NONE',  ( -19.34548696706897175, -4.262109752139091157, 61.51804659027894928 ) ) ;
#12799 = ORIENTED_EDGE ( 'NONE', *, *, #2707, .F. ) ;
#12800 = AXIS2_PLACEMENT_3D ( 'NONE', #14076, #10786, #4827 ) ;
#12801 = DIRECTION ( 'NONE',  ( 0.000000000000000000, 0.000000000000000000, -1.000000000000000000 ) ) ;
#12802 = CIRCLE ( 'NONE', #1548, 2.999999999999999112 ) ;
#12803 = ORIENTED_EDGE ( 'NONE', *, *, #482, .T. ) ;
#12804 = LINE ( 'NONE', #8342, #14052 ) ;
#12805 = LINE ( 'NONE', #7191, #14672 ) ;
#12806 = CIRCLE ( 'NONE', #104, 37.50000000000000000 ) ;
#12807 = EDGE_CURVE ( 'NONE', #14829, #7812, #5775, .T. ) ;
#12808 = LINE ( 'NONE', #12578, #9349 ) ;
#12809 = EDGE_CURVE ( 'NONE', #7737, #7739, #11830, .T. ) ;
#12810 = VERTEX_POINT ( 'NONE', #9380 ) ;
#12811 = CARTESIAN_POINT ( 'NONE',  ( 4.791762596210716652, -37.80121036461403605, -12.03389752085011644 ) ) ;
#12812 = EDGE_LOOP ( 'NONE', ( #3229, #8637, #9216, #12816, #8857, #9337, #11745, #13175 ) ) ;
#12813 = CARTESIAN_POINT ( 'NONE',  ( -7.285742840713465007, -17.36641515085804599, 56.85231026484400019 ) ) ;
#12814 = AXIS2_PLACEMENT_3D ( 'NONE', #11683, #12362, #2873 ) ;
#12815 = EDGE_LOOP ( 'NONE', ( #6479, #1872, #1185, #7060, #13576, #4529, #8911, #11559 ) ) ;
#12816 = ORIENTED_EDGE ( 'NONE', *, *, #7474, .F. ) ;
#12817 = CARTESIAN_POINT ( 'NONE',  ( 4.049098414795642142, -38.38910658709895074, 51.50382295336648752 ) ) ;
#12818 = ORIENTED_EDGE ( 'NONE', *, *, #10701, .F. ) ;
#12819 = CARTESIAN_POINT ( 'NONE',  ( -20.16941728185991423, -22.35032937287301991, 56.71056454896548615 ) ) ;
#12820 = VECTOR ( 'NONE', #3415, 1000.000000000000114 ) ;
#12821 = DIRECTION ( 'NONE',  ( 1.000000000000000000, 0.000000000000000000, 0.000000000000000000 ) ) ;
#12822 = DIRECTION ( 'NONE',  ( 8.018662683283438208E-16, -5.975035461963189015E-16, -1.000000000000000000 ) ) ;
#12823 = EDGE_CURVE ( 'NONE', #13829, #9275, #6431, .T. ) ;
#12824 = EDGE_CURVE ( 'NONE', #745, #12770, #1074, .T. ) ;
#12825 = AXIS2_PLACEMENT_3D ( 'NONE', #4270, #11306, #5489 ) ;
#12826 = DIRECTION ( 'NONE',  ( -0.5196486895212294455, 0.8543800322332379960, -9.271838545667872786E-16 ) ) ;
#12828 = DIRECTION ( 'NONE',  ( -7.070501591499380254E-17, -1.224646799147350002E-16, 1.000000000000000000 ) ) ;
#12827 = CARTESIAN_POINT ( 'NONE',  ( -12.66248504435161948, -4.886969368454929352, 57.00231026484397745 ) ) ;
#12829 = ORIENTED_EDGE ( 'NONE', *, *, #14341, .F. ) ;
#12830 = DIRECTION ( 'NONE',  ( -1.000000000000000000, 1.291538348938060198E-32, -1.054621095516909827E-16 ) ) ;
#12831 = DIRECTION ( 'NONE',  ( 0.000000000000000000, -1.000000000000000000, -1.224646799147350002E-16 ) ) ;
#12832 = ORIENTED_EDGE ( 'NONE', *, *, #9123, .F. ) ;
#12833 = VERTEX_POINT ( 'NONE', #7302 ) ;
#12834 = LINE ( 'NONE', #1190, #8355 ) ;
#12835 = CARTESIAN_POINT ( 'NONE',  ( -22.43956949979004634, -40.49372917221637636, 56.35573215670456193 ) ) ;
#12836 = EDGE_LOOP ( 'NONE', ( #11669, #14921, #9912, #9884 ) ) ;
#12837 =( BOUNDED_CURVE ( )  B_SPLINE_CURVE ( 3, ( #23, #10570, #3533, #10725 ),
 .UNSPECIFIED., .F., .F. ) 
 B_SPLINE_CURVE_WITH_KNOTS ( ( 4, 4 ),
 ( 1.070141614390309526, 1.245066839500267530 ),
 .UNSPECIFIED. ) 
 CURVE ( )  GEOMETRIC_REPRESENTATION_ITEM ( )  RATIONAL_B_SPLINE_CURVE ( ( 1.000000000000000000, 0.9974517222217440526, 0.9974517222217440526, 1.000000000000000000 ) ) 
 REPRESENTATION_ITEM ( '' )  );
#12838 = CARTESIAN_POINT ( 'NONE',  ( -10.62581258585845667, -38.15807761791479180, -17.68017016644601114 ) ) ;
#12839 = VERTEX_POINT ( 'NONE', #4300 ) ;
#12840 = CARTESIAN_POINT ( 'NONE',  ( -15.49969986081099371, -19.50737899243800300, -13.28793577849899599 ) ) ;
#12841 = CONTEXT_DEPENDENT_SHAPE_REPRESENTATION ( #12914, #9700 ) ;
#12842 = DIRECTION ( 'NONE',  ( 0.1272150336605082366, -0.9918751611018171710, 6.946583704589972670E-16 ) ) ;
#12843 = ADVANCED_FACE ( 'NONE', ( #11983 ), #12337, .F. ) ;
#12844 = LINE ( 'NONE', #6992, #9670 ) ;
#12845 = LINE ( 'NONE', #11679, #11586 ) ;
#12846 = EDGE_CURVE ( 'NONE', #3186, #6946, #11187, .T. ) ;
#12847 = ORIENTED_EDGE ( 'NONE', *, *, #4306, .F. ) ;
#12848 = CARTESIAN_POINT ( 'NONE',  ( -10.27578761138057040, -90.55771581991869823, -4.244953887782999757 ) ) ;
#12849 = DIRECTION ( 'NONE',  ( -0.9183863840214729901, -0.3956847857120157075, -4.999999999999999402E-16 ) ) ;
#12850 = CARTESIAN_POINT ( 'NONE',  ( -23.49969986081100259, -44.50737899243799944, -17.13441993860073254 ) ) ;
#12851 = DIRECTION ( 'NONE',  ( -0.5975035461963188466, -0.8018662683283437342, 0.000000000000000000 ) ) ;
#12852 = ORIENTED_EDGE ( 'NONE', *, *, #12335, .T. ) ;
#12853 = DIRECTION ( 'NONE',  ( -1.000000000000000000, 0.000000000000000000, 0.000000000000000000 ) ) ;
#12854 = ORIENTED_EDGE ( 'NONE', *, *, #503, .F. ) ;
#12855 = DIRECTION ( 'NONE',  ( -0.1511109077013120527, -0.9885168150181793401, 4.694715627858928842E-16 ) ) ;
#12856 = CARTESIAN_POINT ( 'NONE',  ( -18.09969986081091164, -110.0073789924380065, -10.19792577984107318 ) ) ;
#12857 = ADVANCED_FACE ( 'NONE', ( #3149 ), #1500, .F. ) ;
#12858 = DIRECTION ( 'NONE',  ( -0.6780482080269578660, -0.7350174335289137995, -1.045284632676540194E-16 ) ) ;
#12859 = AXIS2_PLACEMENT_3D ( 'NONE', #7696, #1742, #8926 ) ;
#12860 = CARTESIAN_POINT ( 'NONE',  ( -15.49969986081100082, -105.5768790231641105, -6.170773065691668613 ) ) ;
#12861 = CARTESIAN_POINT ( 'NONE',  ( -7.719139325354606562, -48.17958124988514612, -7.357509729390519837 ) ) ;
#12862 = CARTESIAN_POINT ( 'NONE',  ( -36.48074150599295962, -37.42264482913270740, 50.58571613516381404 ) ) ;
#12863 = LINE ( 'NONE', #7018, #4972 ) ;
#12864 = ORIENTED_EDGE ( 'NONE', *, *, #6822, .F. ) ;
#12865 = DIRECTION ( 'NONE',  ( 0.7511640317997426708, 0.6601155939154560448, 2.079116908177589032E-16 ) ) ;
#12866 = ORIENTED_EDGE ( 'NONE', *, *, #14766, .F. ) ;
#12868 = ORIENTED_EDGE ( 'NONE', *, *, #10459, .T. ) ;
#12867 = DIRECTION ( 'NONE',  ( 0.5975035461963188466, 0.8018662683283437342, 0.000000000000000000 ) ) ;
#12869 = ORIENTED_EDGE ( 'NONE', *, *, #13659, .T. ) ;
#12870 = DIRECTION ( 'NONE',  ( 0.000000000000000000, 1.000000000000000000, 1.224646799147350002E-16 ) ) ;
#12871 = ORIENTED_EDGE ( 'NONE', *, *, #3136, .T. ) ;
#12872 = AXIS2_PLACEMENT_3D ( 'NONE', #5871, #4591, #8173 ) ;
#12873 = CARTESIAN_POINT ( 'NONE',  ( -16.39856880423293006, -20.52544743201270450, 56.85231026484400019 ) ) ;
#12874 = EDGE_CURVE ( 'NONE', #3314, #13132, #6146, .T. ) ;
#12875 = DIRECTION ( 'NONE',  ( -8.018662683283439195E-16, 5.975035461963190001E-16, 1.000000000000000000 ) ) ;
#12876 = DIRECTION ( 'NONE',  ( 0.9085715390340232123, -0.4177292884839972631, 9.781476007338056784E-16 ) ) ;
#12877 =( NAMED_UNIT ( * ) SI_UNIT ( $, .STERADIAN. ) SOLID_ANGLE_UNIT ( ) );
#12878 = CARTESIAN_POINT ( 'NONE',  ( 18.52103932491873195, -26.54644467364772709, 8.437333501280610548 ) ) ;
#12879 = AXIS2_PLACEMENT_3D ( 'NONE', #3815, #9630, #9781 ) ;
#12880 = CYLINDRICAL_SURFACE ( 'NONE', #2301, 5.250000000000000888 ) ;
#12881 = CARTESIAN_POINT ( 'NONE',  ( -23.49969986081099904, -19.50737899243800300, 54.00231026484400587 ) ) ;
#12882 = CARTESIAN_POINT ( 'NONE',  ( -12.52737422752994156, -16.89904518643017894, -13.17054741830957987 ) ) ;
#12883 = ORIENTED_EDGE ( 'NONE', *, *, #7924, .F. ) ;
#12884 = VERTEX_POINT ( 'NONE', #8530 ) ;
#12885 = AXIS2_PLACEMENT_3D ( 'NONE', #9025, #13704, #3221 ) ;
#12886 = ORIENTED_EDGE ( 'NONE', *, *, #4857, .F. ) ;
#12887 = CARTESIAN_POINT ( 'NONE',  ( 5.757201503570998469, -37.32104008884124369, 50.39558766532553591 ) ) ;
#12888 = VERTEX_POINT ( 'NONE', #8953 ) ;
#12889 = AXIS2_PLACEMENT_3D ( 'NONE', #13226, #7462, #10991 ) ;
#12890 = CARTESIAN_POINT ( 'NONE',  ( -16.42437072798637843, -22.03270794722917714, 56.85231026484400019 ) ) ;
#12891 = EDGE_CURVE ( 'NONE', #9717, #14495, #7656, .T. ) ;
#12892 = AXIS2_PLACEMENT_3D ( 'NONE', #1509, #13225, #8541 ) ;
#12893 = EDGE_CURVE ( 'NONE', #5733, #8005, #3000, .T. ) ;
#12894 = LINE ( 'NONE', #1408, #3423 ) ;
#12895 = CARTESIAN_POINT ( 'NONE',  ( -15.49969986081092088, -13.50737899243822504, 56.85231026484398598 ) ) ;
#12896 = AXIS2_PLACEMENT_3D ( 'NONE', #9620, #14438, #6387 ) ;
#12897 = DIRECTION ( 'NONE',  ( 0.6601155939154559338, -0.7511640317997426708, 9.781476007338054812E-16 ) ) ;
#12899 = DIRECTION ( 'NONE',  ( 0.000000000000000000, 0.000000000000000000, -1.000000000000000000 ) ) ;
#12898 = CARTESIAN_POINT ( 'NONE',  ( 2.500300139189001847, -46.50737899243799944, -5.497689735156002122 ) ) ;
#12900 = ORIENTED_EDGE ( 'NONE', *, *, #11882, .F. ) ;
#12901 = CARTESIAN_POINT ( 'NONE',  ( -17.72286745096104355, -3.783277446994210536, 56.85231026484398598 ) ) ;
#12902 = CIRCLE ( 'NONE', #4594, 0.2000000000000012046 ) ;
#12903 = VECTOR ( 'NONE', #5472, 1000.000000000000000 ) ;
#12904 = CARTESIAN_POINT ( 'NONE',  ( -15.49969986081099371, -18.00737899243799944, -13.28793577849899776 ) ) ;
#12905 = ORIENTED_EDGE ( 'NONE', *, *, #11569, .F. ) ;
#12906 = ORIENTED_EDGE ( 'NONE', *, *, #11099, .T. ) ;
#12907 = CARTESIAN_POINT ( 'NONE',  ( 21.89440327984462442, -28.63919800004179095, 27.03079604377302303 ) ) ;
#12908 = VECTOR ( 'NONE', #1310, 1000.000000000000227 ) ;
#12909 = DIRECTION ( 'NONE',  ( 0.8415927028326188886, -0.5401126942952620968, 9.975640502598240034E-16 ) ) ;
#12910 = EDGE_LOOP ( 'NONE', ( #5683, #12512, #760, #13302 ) ) ;
#12911 = CARTESIAN_POINT ( 'NONE',  ( -13.18491133144367211, -15.23222315862922827, 51.10586365543726117 ) ) ;
#12912 = ORIENTED_EDGE ( 'NONE', *, *, #10931, .T. ) ;
#12913 = EDGE_CURVE ( 'NONE', #6353, #5152, #15011, .T. ) ;
#12914 =( REPRESENTATION_RELATIONSHIP ('NONE','NONE', #2372, #3931 ) REPRESENTATION_RELATIONSHIP_WITH_TRANSFORMATION ( #5631 )SHAPE_REPRESENTATION_RELATIONSHIP( ) );
#12915 = EDGE_CURVE ( 'NONE', #11027, #7413, #3519, .T. ) ;
#12916 = ADVANCED_FACE ( 'NONE', ( #12262 ), #5440, .F. ) ;
#12917 = CARTESIAN_POINT ( 'NONE',  ( -12.87131257180735844, -22.19373785326158099, 56.85231026484400019 ) ) ;
#12918 = CONTEXT_DEPENDENT_SHAPE_REPRESENTATION ( #11037, #6267 ) ;
#12919 = DIRECTION ( 'NONE',  ( -8.018662683283438208E-16, 5.975035461963189015E-16, 1.000000000000000000 ) ) ;
#12920 = EDGE_CURVE ( 'NONE', #9493, #6681, #14354, .T. ) ;
#12921 = LINE ( 'NONE', #60, #3568 ) ;
#12922 = DIRECTION ( 'NONE',  ( 0.8222303661035966771, -0.5691548339926011391, 9.993908270190953088E-16 ) ) ;
#12923 = ORIENTED_EDGE ( 'NONE', *, *, #13561, .T. ) ;
#12924 = CARTESIAN_POINT ( 'NONE',  ( -25.49969986081099904, -13.50737899243799944, 6.712064221500998684 ) ) ;
#12925 = DIRECTION ( 'NONE',  ( -8.018662683283438208E-16, 5.975035461963189015E-16, 1.000000000000000000 ) ) ;
#12926 = ORIENTED_EDGE ( 'NONE', *, *, #10435, .F. ) ;
#12927 = CARTESIAN_POINT ( 'NONE',  ( -24.93814746875458610, -16.73481322911949931, 57.00231026484397745 ) ) ;
#12928 = VERTEX_POINT ( 'NONE', #2823 ) ;
#12929 = AXIS2_PLACEMENT_3D ( 'NONE', #5173, #14514, #12996 ) ;
#12930 = LINE ( 'NONE', #7161, #12557 ) ;
#12931 = VERTEX_POINT ( 'NONE', #9860 ) ;
#12932 = FACE_OUTER_BOUND ( 'NONE', #11112, .T. ) ;
#12933 = DIRECTION ( 'NONE',  ( -8.018662683283438208E-16, 5.975035461963189015E-16, 1.000000000000000000 ) ) ;
#12934 = ADVANCED_FACE ( 'NONE', ( #12961 ), #12880, .F. ) ;
#12935 = EDGE_CURVE ( 'NONE', #9275, #2405, #7405, .T. ) ;
#12936 = DIRECTION ( 'NONE',  ( 0.000000000000000000, -1.000000000000000000, -1.224646799147350002E-16 ) ) ;
#12937 = B_SPLINE_CURVE_WITH_KNOTS ( 'NONE', 3,
 ( #14416, #9673, #6218, #10898, #10971, #3934, #567, #425, #2787, #5232, #4010, #7442, #5303, #11121, #12120, #9895, #14638, #14563, #6293, #641 ),
 .UNSPECIFIED., .F., .F.,
 ( 4, 2, 2, 1, 1, 1, 1, 1, 1, 2, 2, 2, 4 ),
 ( 0.000000000000000000, 0.2500000000006495915, 0.3750000000009743872, 0.4375000000011352030, 0.4687500000012148060, 0.4843750000012558843, 0.4921875000012767565, 0.4960937500012871371, 0.4980468750012915224, 0.4990234375012933543, 0.5000000000012951862, 0.7500000000006475931, 1.000000000000000000 ),
 .UNSPECIFIED. ) ;
#12938 = LINE ( 'NONE', #12703, #5911 ) ;
#12939 = CARTESIAN_POINT ( 'NONE',  ( -23.49969986081099904, -19.50737899243800300, 54.00231026484400587 ) ) ;
#12940 = PRODUCT_DEFINITION_FORMATION_WITH_SPECIFIED_SOURCE ( 'ANY', '', #2011, .NOT_KNOWN. ) ;
#12941 = FACE_BOUND ( 'NONE', #6737, .T. ) ;
#12942 = DIRECTION ( 'NONE',  ( 0.3623424103984807521, -0.9307677159359857288, 0.04877946902055359940 ) ) ;
#12943 = CARTESIAN_POINT ( 'NONE',  ( -9.485644917226064621, -49.78943610649189822, -17.51268299892230829 ) ) ;
#12944 = CARTESIAN_POINT ( 'NONE',  ( -20.68303597405226313, -107.8803405083532567, -6.910450545281812573 ) ) ;
#12945 = EDGE_CURVE ( 'NONE', #8690, #11659, #11098, .T. ) ;
#12946 = ORIENTED_EDGE ( 'NONE', *, *, #3796, .T. ) ;
#12947 = CARTESIAN_POINT ( 'NONE',  ( -8.722797460041883610, -15.53942693735753444, 56.85231026484400019 ) ) ;
#12948 = AXIS2_PLACEMENT_3D ( 'NONE', #11635, #8108, #1154 ) ;
#12949 = ORIENTED_EDGE ( 'NONE', *, *, #3916, .F. ) ;
#12951 = ORIENTED_EDGE ( 'NONE', *, *, #1787, .T. ) ;
#12950 = DIRECTION ( 'NONE',  ( 9.999999999999998805E-16, -0.05233595624294299503, -0.9986295347545739443 ) ) ;
#12952 = VERTEX_POINT ( 'NONE', #179 ) ;
#12953 = AXIS2_PLACEMENT_3D ( 'NONE', #9218, #4646, #4420 ) ;
#12954 = DIRECTION ( 'NONE',  ( 0.000000000000000000, -1.000000000000000000, -1.224646799147350002E-16 ) ) ;
#12955 = ORIENTED_EDGE ( 'NONE', *, *, #1121, .F. ) ;
#12956 = LINE ( 'NONE', #2463, #5595 ) ;
#12957 = CARTESIAN_POINT ( 'NONE',  ( -7.785174720008381399, -8.727488632615573394, 57.00231026484399166 ) ) ;
#12958 = DIRECTION ( 'NONE',  ( 0.5975035461963189576, 0.8018662683283437342, 0.000000000000000000 ) ) ;
#12959 = CARTESIAN_POINT ( 'NONE',  ( -6.368730986314239395, -9.491655842995189829, 56.85231026484400019 ) ) ;
#12960 = CIRCLE ( 'NONE', #14862, 9.974999999999999645 ) ;
#12961 = FACE_OUTER_BOUND ( 'NONE', #5311, .T. ) ;
#12962 = EDGE_CURVE ( 'NONE', #15034, #12656, #12081, .T. ) ;
#12963 = DIRECTION ( 'NONE',  ( -1.927249326158839857E-15, 1.000000000000000000, 0.000000000000000000 ) ) ;
#12964 = CARTESIAN_POINT ( 'NONE',  ( -11.22942933597135706, -14.95710884211384695, -13.04417926711732356 ) ) ;
#12965 = ORIENTED_EDGE ( 'NONE', *, *, #11028, .T. ) ;
#12966 =( NAMED_UNIT ( * ) SI_UNIT ( $, .STERADIAN. ) SOLID_ANGLE_UNIT ( ) );
#12967 = VERTEX_POINT ( 'NONE', #526 ) ;
#12968 = ORIENTED_EDGE ( 'NONE', *, *, #13552, .F. ) ;
#12969 = CARTESIAN_POINT ( 'NONE',  ( 7.500300139189000070, -37.00737899243799944, 49.12071670408379731 ) ) ;
#12970 = EDGE_LOOP ( 'NONE', ( #5058, #8043, #2339, #8728 ) ) ;
#12971 = DIRECTION ( 'NONE',  ( -8.018662683283438208E-16, 5.975035461963189015E-16, 1.000000000000000000 ) ) ;
#12972 = SURFACE_STYLE_FILL_AREA ( #350 ) ;
#12973 = CARTESIAN_POINT ( 'NONE',  ( 22.00030013918900096, -27.00737899243800300, 43.21206422150100224 ) ) ;
#12974 = AXIS2_PLACEMENT_3D ( 'NONE', #7283, #11969, #3075 ) ;
#12975 = CARTESIAN_POINT ( 'NONE',  ( -15.49969986081099371, -23.50737899243800300, 56.85231026484400019 ) ) ;
#12976 = EDGE_CURVE ( 'NONE', #6551, #15009, #13317, .T. ) ;
#12978 = DIRECTION ( 'NONE',  ( 0.000000000000000000, 1.000000000000000000, 1.224646799147350002E-16 ) ) ;
#12977 = DIRECTION ( 'NONE',  ( -1.000000000000000000, -1.201369187114119994E-15, -9.616040805000176517E-16 ) ) ;
#12979 = ORIENTED_EDGE ( 'NONE', *, *, #9826, .T. ) ;
#12980 = CARTESIAN_POINT ( 'NONE',  ( -15.49969986081099904, -107.1622034095870077, -6.087689735155999315 ) ) ;
#12981 = DIRECTION ( 'NONE',  ( -0.9885168150181790070, 0.1511109077013141622, -8.829475928589267021E-16 ) ) ;
#12982 = VERTEX_POINT ( 'NONE', #4046 ) ;
#12983 = ORIENTED_EDGE ( 'NONE', *, *, #4947, .T. ) ;
#12984 = CARTESIAN_POINT ( 'NONE',  ( -33.49969986081099904, -37.00737899243799944, -13.39525803434800011 ) ) ;
#12985 = CARTESIAN_POINT ( 'NONE',  ( -15.49969986081092088, -13.50737899243822504, 56.85231026484398598 ) ) ;
#12986 = VERTEX_POINT ( 'NONE', #12086 ) ;
#12987 = DIRECTION ( 'NONE',  ( 0.05771543059946733500, -0.9983330752162417054, 6.427876096865391919E-16 ) ) ;
#12988 = CARTESIAN_POINT ( 'NONE',  ( -5.499699860811003482, -46.50737899243799944, 47.50231026484399877 ) ) ;
#12989 = AXIS2_PLACEMENT_3D ( 'NONE', #2936, #5150, #10970 ) ;
#12990 = LINE ( 'NONE', #12763, #2151 ) ;
#12991 = CARTESIAN_POINT ( 'NONE',  ( -21.68801466096620700, -19.44379288755867208, 56.85231026484398598 ) ) ;
#12992 = ADVANCED_FACE ( 'NONE', ( #4844 ), #14093, .T. ) ;
#12993 = CARTESIAN_POINT ( 'NONE',  ( -7.821737630532772378, -18.34578224045527151, 56.85231026484400019 ) ) ;
#12994 = VERTEX_POINT ( 'NONE', #5191 ) ;
#12995 = DIRECTION ( 'NONE',  ( -1.054621095516909827E-16, -1.224646799147350002E-16, 1.000000000000000000 ) ) ;
#12996 = DIRECTION ( 'NONE',  ( 0.5975035461963189576, 0.8018662683283437342, 0.000000000000000000 ) ) ;
#12997 = ORIENTED_EDGE ( 'NONE', *, *, #9574, .F. ) ;
#12998 = EDGE_CURVE ( 'NONE', #8928, #9118, #6435, .T. ) ;
#12999 = CARTESIAN_POINT ( 'NONE',  ( -7.691420491076302213, -11.44776172600821340, 57.00231026484399166 ) ) ;
#13000 = ORIENTED_EDGE ( 'NONE', *, *, #4454, .F. ) ;
#13001 = LINE ( 'NONE', #11841, #6912 ) ;
#13002 = ORIENTED_EDGE ( 'NONE', *, *, #934, .F. ) ;
#13003 = AXIS2_PLACEMENT_3D ( 'NONE', #2452, #12865, #239 ) ;
#13004 = CARTESIAN_POINT ( 'NONE',  ( 1.760741030006599317, 10.68321993080349763, 32.15417856559049881 ) ) ;
#13005 = LINE ( 'NONE', #2443, #4115 ) ;
#13006 = CARTESIAN_POINT ( 'NONE',  ( -22.33089034576175180, -8.323646113680169378, 56.85231026484398598 ) ) ;
#13007 = EDGE_CURVE ( 'NONE', #1679, #2810, #4016, .T. ) ;
#13008 = DIRECTION ( 'NONE',  ( 0.000000000000000000, 1.224646799147350002E-16, -1.000000000000000000 ) ) ;
#13009 = LINE ( 'NONE', #3437, #7679 ) ;
#13010 = CARTESIAN_POINT ( 'NONE',  ( -6.194530427787681148, -17.17519237421424094, 60.53940394396870062 ) ) ;
#13011 = VECTOR ( 'NONE', #12909, 1000.000000000000114 ) ;
#13012 = EDGE_CURVE ( 'NONE', #2455, #12888, #5956, .T. ) ;
#13013 = AXIS2_PLACEMENT_3D ( 'NONE', #2345, #9212, #14891 ) ;
#13014 = AXIS2_PLACEMENT_3D ( 'NONE', #3965, #1367, #13008 ) ;
#13015 = CARTESIAN_POINT ( 'NONE',  ( 16.67641871555605348, -30.25287370156248912, 4.950703260674607975 ) ) ;
#13016 = EDGE_CURVE ( 'NONE', #6590, #4359, #3973, .T. ) ;
#13017 = ORIENTED_EDGE ( 'NONE', *, *, #12630, .T. ) ;
#13018 = CARTESIAN_POINT ( 'NONE',  ( -13.68042463183279089, -52.30222829753689950, -17.95442675827648316 ) ) ;
#13019 = ADVANCED_FACE ( 'NONE', ( #9423 ), #1239, .T. ) ;
#13020 = CARTESIAN_POINT ( 'NONE',  ( -35.22389609106763686, -38.22985747236961629, 51.39598352406615334 ) ) ;
#13021 = DIRECTION ( 'NONE',  ( 8.660254037844387408E-16, -0.8660254037844387076, 0.4999999999999998890 ) ) ;
#13022 = ORIENTED_EDGE ( 'NONE', *, *, #6985, .F. ) ;
#13023 = DIRECTION ( 'NONE',  ( -8.018662683283438208E-16, 5.975035461963189015E-16, 1.000000000000000000 ) ) ;
#13024 = ORIENTED_EDGE ( 'NONE', *, *, #2855, .F. ) ;
#13026 = ORIENTED_EDGE ( 'NONE', *, *, #5145, .F. ) ;
#13025 = DIRECTION ( 'NONE',  ( 8.018662683283438208E-16, -5.975035461963189015E-16, -1.000000000000000000 ) ) ;
#13027 = EDGE_LOOP ( 'NONE', ( #8964, #14364, #6335, #5754 ) ) ;
#13028 = DIRECTION ( 'NONE',  ( 1.000000000000000000, 1.499759782661853776E-32, -1.224646799147353207E-16 ) ) ;
#13029 = EDGE_LOOP ( 'NONE', ( #7232, #9867, #8313, #4768 ) ) ;
#13030 = AXIS2_PLACEMENT_3D ( 'NONE', #3110, #11150, #14668 ) ;
#13031 = CARTESIAN_POINT ( 'NONE',  ( 7.500300139189000070, -42.00737899243800655, 19.50231026484400587 ) ) ;
#13032 = AXIS2_PLACEMENT_3D ( 'NONE', #7960, #5675, #1163 ) ;
#13033 = FACE_OUTER_BOUND ( 'NONE', #11074, .T. ) ;
#13034 = LINE ( 'NONE', #10800, #11255 ) ;
#13035 = CARTESIAN_POINT ( 'NONE',  ( -16.10498554648964387, -101.6262671406525016, -6.037303569837844108 ) ) ;
#13036 = EDGE_CURVE ( 'NONE', #186, #9490, #8555, .T. ) ;
#13037 = CIRCLE ( 'NONE', #3496, 9.974999999999999645 ) ;
#13038 = DIRECTION ( 'NONE',  ( 0.000000000000000000, 0.1872998510044495413, 0.9823027872370673208 ) ) ;
#13039 = ADVANCED_FACE ( 'NONE', ( #2750 ), #1596, .F. ) ;
#13040 = CARTESIAN_POINT ( 'NONE',  ( 2.638979504099960405, -40.83713880673332142, -13.31900631518413824 ) ) ;
#13041 = ORIENTED_EDGE ( 'NONE', *, *, #1865, .F. ) ;
#13042 = ORIENTED_EDGE ( 'NONE', *, *, #12141, .F. ) ;
#13043 = EDGE_LOOP ( 'NONE', ( #4985, #9621, #12071, #1441 ) ) ;
#13044 = FACE_OUTER_BOUND ( 'NONE', #3394, .T. ) ;
#13045 = EDGE_LOOP ( 'NONE', ( #9926, #12095, #4613, #983 ) ) ;
#13046 = CARTESIAN_POINT ( 'NONE',  ( -7.499699860810999041, -19.50737899243799589, 54.00231026484400587 ) ) ;
#13047 = CARTESIAN_POINT ( 'NONE',  ( -15.49969986081099727, -36.50737899243799944, 2.502310264843996546 ) ) ;
#13048 = EDGE_CURVE ( 'NONE', #5828, #5586, #4690, .T. ) ;
#13049 = CARTESIAN_POINT ( 'NONE',  ( -18.09969986081100046, -107.1622034095870077, -6.087689735156001980 ) ) ;
#13050 = DIRECTION ( 'NONE',  ( 0.000000000000000000, 1.224646799147350002E-16, -1.000000000000000000 ) ) ;
#13051 = VECTOR ( 'NONE', #14040, 1000.000000000000000 ) ;
#13052 = AXIS2_PLACEMENT_3D ( 'NONE', #10366, #12831, #4714 ) ;
#13053 = FACE_OUTER_BOUND ( 'NONE', #10526, .T. ) ;
#13054 = DIRECTION ( 'NONE',  ( 1.000000000000000000, -1.291538348938060198E-32, 1.054621095516909827E-16 ) ) ;
#13055 = VERTEX_POINT ( 'NONE', #3614 ) ;
#13056 = LINE ( 'NONE', #10748, #6288 ) ;
#13057 = PLANE ( 'NONE',  #7880 ) ;
#13058 = EDGE_LOOP ( 'NONE', ( #9175, #3355 ) ) ;
#13059 = ORIENTED_EDGE ( 'NONE', *, *, #4928, .F. ) ;
#13060 = VECTOR ( 'NONE', #3896, 1000.000000000000000 ) ;
#13061 = CARTESIAN_POINT ( 'NONE',  ( -22.68580030561789940, -40.95256572998779632, 56.30791217491542966 ) ) ;
#13062 = ORIENTED_EDGE ( 'NONE', *, *, #14726, .T. ) ;
#13063 = CARTESIAN_POINT ( 'NONE',  ( -10.02866676776782917, -38.66483879159430614, -17.59691272929029893 ) ) ;
#13064 = VECTOR ( 'NONE', #15051, 1000.000000000000114 ) ;
#13065 = EDGE_CURVE ( 'NONE', #3452, #3490, #7112, .T. ) ;
#13066 = CARTESIAN_POINT ( 'NONE',  ( -15.49969986081099904, -57.00737899243800655, 19.50231026484399877 ) ) ;
#13067 = AXIS2_PLACEMENT_3D ( 'NONE', #7586, #8807, #632 ) ;
#13068 = CYLINDRICAL_SURFACE ( 'NONE', #10202, 3.250000000000002665 ) ;
#13069 = DIRECTION ( 'NONE',  ( 0.000000000000000000, -1.000000000000000000, -1.224646799147350002E-16 ) ) ;
#13070 = CARTESIAN_POINT ( 'NONE',  ( -15.49969986081099194, -27.00737899243800300, 19.50231026484399877 ) ) ;
#13071 = VERTEX_POINT ( 'NONE', #10572 ) ;
#13072 = CARTESIAN_POINT ( 'NONE',  ( -1.821162622431176770, -49.50737899243799944, -5.497689735156000346 ) ) ;
#13073 = CARTESIAN_POINT ( 'NONE',  ( -11.30335942247960546, -22.55676305576680818, 57.00231026484399166 ) ) ;
#13074 = EDGE_LOOP ( 'NONE', ( #974, #8603, #5112, #14098, #2828 ) ) ;
#13075 = DIRECTION ( 'NONE',  ( 0.000000000000000000, 1.700257036304450134E-17, -1.000000000000000000 ) ) ;
#13076 = PRESENTATION_STYLE_ASSIGNMENT (( #8622 ) ) ;
#13077 = ORIENTED_EDGE ( 'NONE', *, *, #9667, .F. ) ;
#13078 = CARTESIAN_POINT ( 'NONE',  ( -7.510805671289423557, -44.08454136026598746, -6.142818529867362543 ) ) ;
#13079 = ORIENTED_EDGE ( 'NONE', *, *, #9532, .F. ) ;
#13080 = AXIS2_PLACEMENT_3D ( 'NONE', #4589, #2371, #155 ) ;
#13081 = CARTESIAN_POINT ( 'NONE',  ( -22.58324314276470091, -9.630648466248954875, 57.00231026484397745 ) ) ;
#13082 = PLANE ( 'NONE',  #9156 ) ;
#13083 = EDGE_CURVE ( 'NONE', #4089, #15030, #11796, .T. ) ;
#13084 = DIRECTION ( 'NONE',  ( 0.8357240892757724637, 0.5491495666976170531, 3.420201433256690644E-16 ) ) ;
#13085 = EDGE_CURVE ( 'NONE', #10077, #13839, #832, .T. ) ;
#13086 = CARTESIAN_POINT ( 'NONE',  ( -15.12969879992303746, -10.35358246313022335, 57.00231026484397745 ) ) ;
#13087 = AXIS2_PLACEMENT_3D ( 'NONE', #5278, #3911, #8567 ) ;
#13088 = CARTESIAN_POINT ( 'NONE',  ( -12.66248504435161948, -4.886969368454929352, 56.85231026484398598 ) ) ;
#13089 = CARTESIAN_POINT ( 'NONE',  ( -5.615565924346643811, -12.16405426399944112, 54.00231026484399166 ) ) ;
#13090 = CARTESIAN_POINT ( 'NONE',  ( -34.15367539102294359, -39.53260173292695612, 52.03355220560322181 ) ) ;
#13091 = FACE_OUTER_BOUND ( 'NONE', #2793, .T. ) ;
#13092 = VERTEX_POINT ( 'NONE', #1901 ) ;
#13093 = PLANE ( 'NONE',  #8089 ) ;
#13094 = ORIENTED_EDGE ( 'NONE', *, *, #6545, .F. ) ;
#13096 = EDGE_LOOP ( 'NONE', ( #8354, #14168, #3677, #9538 ) ) ;
#13095 = PLANE ( 'NONE',  #4725 ) ;
#13097 = ORIENTED_EDGE ( 'NONE', *, *, #2103, .T. ) ;
#13098 = DIRECTION ( 'NONE',  ( -0.8160499452489514693, -0.5779813897169900905, -3.090169943749478258E-16 ) ) ;
#13099 = ORIENTED_EDGE ( 'NONE', *, *, #4117, .F. ) ;
#13100 = EDGE_CURVE ( 'NONE', #1960, #8293, #1826, .T. ) ;
#13101 = EDGE_CURVE ( 'NONE', #11705, #3567, #11836, .T. ) ;
#13102 = DIRECTION ( 'NONE',  ( 0.7350174335289111349, -0.6780482080269607525, 9.945218953682729003E-16 ) ) ;
#13103 =( BOUNDED_CURVE ( )  B_SPLINE_CURVE ( 3, ( #7790, #694, #1920, #4440 ),
 .UNSPECIFIED., .F., .T. ) 
 B_SPLINE_CURVE_WITH_KNOTS ( ( 4, 4 ),
 ( 1.570796326794896114, 3.141592653589792672 ),
 .UNSPECIFIED. ) 
 CURVE ( )  GEOMETRIC_REPRESENTATION_ITEM ( )  RATIONAL_B_SPLINE_CURVE ( ( 1.000000000000000000, 0.8047378541243649375, 0.8047378541243649375, 1.000000000000000000 ) ) 
 REPRESENTATION_ITEM ( '' )  );
#13104 = VECTOR ( 'NONE', #12380, 1000.000000000000000 ) ;
#13105 = EDGE_CURVE ( 'NONE', #6446, #626, #674, .T. ) ;
#13106 = CARTESIAN_POINT ( 'NONE',  ( -15.47724068538499154, -13.46270701644446177, 56.85231026484398598 ) ) ;
#13107 = SHAPE_REPRESENTATION_RELATIONSHIP ( 'NONE' , 'NONE' ,  #2852, #76 ) ;
#13108 = CARTESIAN_POINT ( 'NONE',  ( -18.88793338163855751, -10.53151576015236657, -13.13513322929154725 ) ) ;
#13109 = EDGE_CURVE ( 'NONE', #1528, #1516, #6550, .T. ) ;
#13110 = LINE ( 'NONE', #11955, #326 ) ;
#13111 = APPLICATION_CONTEXT ( 'automotive_design' ) ;
#13112 = CARTESIAN_POINT ( 'NONE',  ( -11.14430855146604316, -14.67662645734702842, -13.03419638460520069 ) ) ;
#13113 = ORIENTED_EDGE ( 'NONE', *, *, #7126, .T. ) ;
#13114 = CIRCLE ( 'NONE', #9429, 9.974999999999999645 ) ;
#13115 = CARTESIAN_POINT ( 'NONE',  ( -12.91190996461674168, -5.858263458394094236, 57.00231026484397745 ) ) ;
#13116 = FACE_OUTER_BOUND ( 'NONE', #12910, .T. ) ;
#13117 = VERTEX_POINT ( 'NONE', #3119 ) ;
#13118 = ORIENTED_EDGE ( 'NONE', *, *, #8128, .T. ) ;
#13119 = LINE ( 'NONE', #2625, #14461 ) ;
#13120 = ORIENTED_EDGE ( 'NONE', *, *, #3690, .F. ) ;
#13121 = DIRECTION ( 'NONE',  ( 0.000000000000000000, 0.000000000000000000, 1.000000000000000000 ) ) ;
#13122 = DIRECTION ( 'NONE',  ( 0.7737441449604661736, 0.6334982226805353500, 2.419218955996689845E-16 ) ) ;
#13123 = ADVANCED_FACE ( 'NONE', ( #12461 ), #5341, .T. ) ;
#13124 = EDGE_CURVE ( 'NONE', #9738, #2929, #6699, .T. ) ;
#13125 = DIRECTION ( 'NONE',  ( 1.169602638241521591E-15, -0.1872998510044552312, -0.9823027872370662106 ) ) ;
#13126 = DIRECTION ( 'NONE',  ( 0.000000000000000000, 1.000000000000000000, 1.224646799147350002E-16 ) ) ;
#13127 = VECTOR ( 'NONE', #1687, 1000.000000000000114 ) ;
#13128 = MECHANICAL_DESIGN_GEOMETRIC_PRESENTATION_REPRESENTATION (  '', ( #7235 ), #12645 ) ;
#13129 = FACE_OUTER_BOUND ( 'NONE', #3061, .T. ) ;
#13131 = CARTESIAN_POINT ( 'NONE',  ( -11.08622897860377954, -4.561882931743225456, 57.00231026484397745 ) ) ;
#13130 = DIRECTION ( 'NONE',  ( 8.018662683283438208E-16, -5.975035461963189015E-16, -1.000000000000000000 ) ) ;
#13132 = VERTEX_POINT ( 'NONE', #4193 ) ;
#13133 = LINE ( 'NONE', #11977, #14375 ) ;
#13134 = CARTESIAN_POINT ( 'NONE',  ( -32.76014075162859740, 10.68321993080349763, 32.15417856559049881 ) ) ;
#13135 = VERTEX_POINT ( 'NONE', #8852 ) ;
#13136 = ORIENTED_EDGE ( 'NONE', *, *, #14468, .F. ) ;
#13137 = EDGE_CURVE ( 'NONE', #8177, #2827, #2966, .T. ) ;
#13138 = LINE ( 'NONE', #7299, #6634 ) ;
#13139 = CONICAL_SURFACE ( 'NONE', #15063, 8.314203600725839749, 0.8578293273552097808 ) ;
#13140 = ORIENTED_EDGE ( 'NONE', *, *, #12079, .F. ) ;
#13141 = DIRECTION ( 'NONE',  ( 0.5975035461963189576, 0.8018662683283437342, 0.000000000000000000 ) ) ;
#13142 = VECTOR ( 'NONE', #622, 1000.000000000000000 ) ;
#13143 = DIRECTION ( 'NONE',  ( 0.000000000000000000, -1.000000000000000000, -1.224646799147350002E-16 ) ) ;
#13144 = DIRECTION ( 'NONE',  ( 0.000000000000000000, 1.508455196501571429E-16, -1.000000000000000000 ) ) ;
#13145 = CIRCLE ( 'NONE', #5312, 37.50000000000000000 ) ;
#13146 = CYLINDRICAL_SURFACE ( 'NONE', #5038, 6.250000000000001776 ) ;
#13147 = DIRECTION ( 'NONE',  ( 0.000000000000000000, -1.000000000000000000, -1.224646799147350002E-16 ) ) ;
#13148 = AXIS2_PLACEMENT_3D ( 'NONE', #4605, #12954, #15078 ) ;
#13149 = ORIENTED_EDGE ( 'NONE', *, *, #14971, .T. ) ;
#13150 = CARTESIAN_POINT ( 'NONE',  ( -20.61203582816999713, -107.3495032605914616, -7.069992522393072854 ) ) ;
#13151 = CARTESIAN_POINT ( 'NONE',  ( -9.989347722329677381, -43.50737899243799944, -5.497689735156000346 ) ) ;
#13152 = ORIENTED_EDGE ( 'NONE', *, *, #9575, .F. ) ;
#13153 = EDGE_CURVE ( 'NONE', #10559, #3186, #13532, .T. ) ;
#13154 = CARTESIAN_POINT ( 'NONE',  ( -31.79969986081099975, 11.99262100756199878, 24.26206422150100650 ) ) ;
#13155 =( NAMED_UNIT ( * ) PLANE_ANGLE_UNIT ( ) SI_UNIT ( $, .RADIAN. ) );
#13156 = VERTEX_POINT ( 'NONE', #3197 ) ;
#13157 = CARTESIAN_POINT ( 'NONE',  ( -19.05456510292772876, -4.187316862259577555, 57.00231026484397745 ) ) ;
#13158 = ORIENTED_EDGE ( 'NONE', *, *, #1293, .F. ) ;
#13159 = CARTESIAN_POINT ( 'NONE',  ( -15.49969986081092088, -13.50737899243822504, 56.85231026484398598 ) ) ;
#13160 = VECTOR ( 'NONE', #12830, 1000.000000000000000 ) ;
#13161 = AXIS2_PLACEMENT_3D ( 'NONE', #14957, #13591, #14805 ) ;
#13162 = VECTOR ( 'NONE', #7641, 1000.000000000000000 ) ;
#13163 = CYLINDRICAL_SURFACE ( 'NONE', #13987, 0.2000000000000012046 ) ;
#13164 = CARTESIAN_POINT ( 'NONE',  ( -7.836123178633778608, -47.48973556348496317, 17.20209991677158357 ) ) ;
#13165 = CARTESIAN_POINT ( 'NONE',  ( 15.51501874267047576, -29.51299105794866051, 3.131973333163219131 ) ) ;
#13166 = EDGE_LOOP ( 'NONE', ( #12979, #3347, #14498, #3338 ) ) ;
#13167 = DIRECTION ( 'NONE',  ( -0.2301973227387161258, 0.9731439732146150989, -7.660444431189777453E-16 ) ) ;
#13168 = DIRECTION ( 'NONE',  ( -0.3956847857120157075, 0.9183863840214729901, -8.660254037844387408E-16 ) ) ;
#13169 = CARTESIAN_POINT ( 'NONE',  ( -15.49969986081099904, -52.50737899243800655, -13.49768973515600656 ) ) ;
#13170 = EDGE_CURVE ( 'NONE', #12295, #13665, #4425, .T. ) ;
#13171 = ORIENTED_EDGE ( 'NONE', *, *, #13835, .F. ) ;
#13172 = CARTESIAN_POINT ( 'NONE',  ( -16.26465502354534465, -4.464365468230401923, 56.85231026484398598 ) ) ;
#13173 = EDGE_LOOP ( 'NONE', ( #13502, #12019, #5371, #399 ) ) ;
#13175 = ORIENTED_EDGE ( 'NONE', *, *, #6730, .F. ) ;
#13174 = CARTESIAN_POINT ( 'NONE',  ( -33.49969986081099904, -42.00737899243800655, -13.39525803434800011 ) ) ;
#13176 = ORIENTED_EDGE ( 'NONE', *, *, #4789, .F. ) ;
#13177 = EDGE_CURVE ( 'NONE', #1021, #10935, #6471, .T. ) ;
#13178 = CARTESIAN_POINT ( 'NONE',  ( -10.22560374232860347, -19.62253721876480483, 56.85231026484400019 ) ) ;
#13179 = VERTEX_POINT ( 'NONE', #754 ) ;
#13180 = DIRECTION ( 'NONE',  ( 0.5975035461963188466, 0.8018662683283438453, 0.000000000000000000 ) ) ;
#13181 = DIRECTION ( 'NONE',  ( -1.734723475976805615E-16, 0.000000000000000000, 1.000000000000000000 ) ) ;
#13182 =( NAMED_UNIT ( * ) PLANE_ANGLE_UNIT ( ) SI_UNIT ( $, .RADIAN. ) );
#13183 = CARTESIAN_POINT ( 'NONE',  ( -18.15085299098534577, -14.64962258016358199, 56.75231026484397745 ) ) ;
#13184 = VECTOR ( 'NONE', #325, 1000.000000000000114 ) ;
#13185 = AXIS2_PLACEMENT_3D ( 'NONE', #5973, #11793, #1319 ) ;
#13186 = DIRECTION ( 'NONE',  ( 0.000000000000000000, 0.000000000000000000, 1.000000000000000000 ) ) ;
#13187 = EDGE_CURVE ( 'NONE', #10716, #5664, #4265, .T. ) ;
#13188 = CARTESIAN_POINT ( 'NONE',  ( -7.654212976755197850, -10.04550297615607768, 57.00231026484399166 ) ) ;
#13189 = EDGE_CURVE ( 'NONE', #14941, #9624, #10145, .T. ) ;
#13190 = VERTEX_POINT ( 'NONE', #4352 ) ;
#13191 = CARTESIAN_POINT ( 'NONE',  ( -7.711221940648826489, -11.37542292179617753, 57.00231026484399166 ) ) ;
#13192 = DIRECTION ( 'NONE',  ( 0.000000000000000000, 0.000000000000000000, 1.000000000000000000 ) ) ;
#13193 = ORIENTED_EDGE ( 'NONE', *, *, #9548, .T. ) ;
#13194 = VERTEX_POINT ( 'NONE', #9002 ) ;
#13195 = EDGE_CURVE ( 'NONE', #1146, #13135, #13681, .T. ) ;
#13196 = DIRECTION ( 'NONE',  ( 0.000000000000000000, 1.850371707708594316E-16, -1.000000000000000000 ) ) ;
#13197 = VERTEX_POINT ( 'NONE', #9076 ) ;
#13198 = ORIENTED_EDGE ( 'NONE', *, *, #12998, .F. ) ;
#13199 = CARTESIAN_POINT ( 'NONE',  ( -12.81093390292747536, -9.898980784960684787, 48.00231026484398456 ) ) ;
#13200 = VECTOR ( 'NONE', #7801, 1000.000000000000000 ) ;
#13201 = EDGE_CURVE ( 'NONE', #12931, #7197, #13755, .T. ) ;
#13202 = CIRCLE ( 'NONE', #1949, 0.4500000000000011768 ) ;
#13203 = CARTESIAN_POINT ( 'NONE',  ( -14.04486373469046434, -92.52292627908343547, -10.69836684062160437 ) ) ;
#13204 = APPLICATION_CONTEXT ( 'automotive_design' ) ;
#13205 = DIRECTION ( 'NONE',  ( 1.000000000000000000, 0.000000000000000000, 0.000000000000000000 ) ) ;
#13207 = DIRECTION ( 'NONE',  ( -1.000000000000000000, -1.201369187114119994E-15, -9.616040805000176517E-16 ) ) ;
#13206 = DIRECTION ( 'NONE',  ( 0.6601155939154559338, -0.7511640317997426708, 9.781476007338054812E-16 ) ) ;
#13208 = ADVANCED_FACE ( 'NONE', ( #1743 ), #6400, .T. ) ;
#13209 = ORIENTED_EDGE ( 'NONE', *, *, #1013, .T. ) ;
#13210 = CARTESIAN_POINT ( 'NONE',  ( -23.49969986081099904, -44.50737899243799944, 19.50231026484399877 ) ) ;
#13211 = ADVANCED_FACE ( 'NONE', ( #15046 ), #1272, .F. ) ;
#13212 = CARTESIAN_POINT ( 'NONE',  ( -23.49969986081099904, -44.50737899243799944, -5.497689735156002122 ) ) ;
#13213 = VERTEX_POINT ( 'NONE', #5712 ) ;
#13214 = VERTEX_POINT ( 'NONE', #3422 ) ;
#13215 = CARTESIAN_POINT ( 'NONE',  ( -23.49969986081100259, -44.50737899243799944, 56.13904046828872652 ) ) ;
#13216 = EDGE_LOOP ( 'NONE', ( #7396, #6797 ) ) ;
#13217 = CARTESIAN_POINT ( 'NONE',  ( 1.935382057079082951, 9.209028802368010247, 16.66098455162964953 ) ) ;
#13218 = CIRCLE ( 'NONE', #11246, 15.87500000000000355 ) ;
#13219 = DIRECTION ( 'NONE',  ( 0.000000000000000000, 1.224646799147350002E-16, -1.000000000000000000 ) ) ;
#13220 = CARTESIAN_POINT ( 'NONE',  ( -15.80242800153736837, -16.08775797096295435, 51.00231026484399166 ) ) ;
#13221 = DIRECTION ( 'NONE',  ( -0.7276687409742212953, -0.6859287159822015090, -1.736481776669299976E-16 ) ) ;
#13222 = CARTESIAN_POINT ( 'NONE',  ( -15.49969986081092088, -13.50737899243822504, 57.00231026484397745 ) ) ;
#13224 = ORIENTED_EDGE ( 'NONE', *, *, #10180, .F. ) ;
#13223 = AXIS2_PLACEMENT_3D ( 'NONE', #4762, #10495, #8111 ) ;
#13225 = DIRECTION ( 'NONE',  ( 1.000000000000000078E-15, -1.000000000000000000, 0.000000000000000000 ) ) ;
#13226 = CARTESIAN_POINT ( 'NONE',  ( -15.53979317422733786, -13.47750381512840967, 56.85231026484398598 ) ) ;
#13227 = VERTEX_POINT ( 'NONE', #1123 ) ;
#13228 = CARTESIAN_POINT ( 'NONE',  ( -6.758527451664999575, -46.50737899243799944, -5.497689735156000346 ) ) ;
#13229 = CARTESIAN_POINT ( 'NONE',  ( -14.61203582816999891, -107.9994814593942607, -7.057848339359947154 ) ) ;
#13230 = VERTEX_POINT ( 'NONE', #9227 ) ;
#13231 = CARTESIAN_POINT ( 'NONE',  ( -15.51120972694785749, -13.45872179377749589, 56.85231026484398598 ) ) ;
#13232 = ORIENTED_EDGE ( 'NONE', *, *, #3831, .T. ) ;
#13233 = DIRECTION ( 'NONE',  ( 8.018662683283438208E-16, -5.975035461963189015E-16, -1.000000000000000000 ) ) ;
#13234 = LINE ( 'NONE', #4814, #618 ) ;
#13235 = LINE ( 'NONE', #2743, #7122 ) ;
#13236 = EDGE_CURVE ( 'NONE', #11256, #11705, #11607, .T. ) ;
#13237 = EDGE_CURVE ( 'NONE', #11236, #12600, #12845, .T. ) ;
#13238 = CARTESIAN_POINT ( 'NONE',  ( -7.503901077028573674, -48.99487332462108213, 19.24414095425641946 ) ) ;
#13239 = CARTESIAN_POINT ( 'NONE',  ( 14.68618260102867445, -27.23672126206158239, 1.962064221501001571 ) ) ;
#13240 = CARTESIAN_POINT ( 'NONE',  ( -15.49969986081099904, 37.56536188261469533, 24.21206422150100224 ) ) ;
#13241 = ORIENTED_EDGE ( 'NONE', *, *, #9892, .T. ) ;
#13242 = CARTESIAN_POINT ( 'NONE',  ( -10.21329888696127419, -50.53437901354443085, -17.62507332399013293 ) ) ;
#13243 = CARTESIAN_POINT ( 'NONE',  ( -18.68395610307571530, -20.92841410781112899, 57.00231026484397745 ) ) ;
#13244 = AXIS2_PLACEMENT_3D ( 'NONE', #13279, #11197, #3159 ) ;
#13245 = VERTEX_POINT ( 'NONE', #11750 ) ;
#13246 = FACE_OUTER_BOUND ( 'NONE', #10580, .T. ) ;
#13247 = ORIENTED_EDGE ( 'NONE', *, *, #14282, .F. ) ;
#13249 = ORIENTED_EDGE ( 'NONE', *, *, #3539, .F. ) ;
#13248 = CARTESIAN_POINT ( 'NONE',  ( -33.58068771901564276, -41.10853556843252221, -13.35081987796131031 ) ) ;
#13250 = ORIENTED_EDGE ( 'NONE', *, *, #6811, .F. ) ;
#13251 = CARTESIAN_POINT ( 'NONE',  ( -22.56290636796585503, -13.91571566392944526, 57.00231026484397745 ) ) ;
#13252 = CARTESIAN_POINT ( 'NONE',  ( -15.49969986081100259, -19.50737899243800300, 54.00231026484400587 ) ) ;
#13253 = AXIS2_PLACEMENT_3D ( 'NONE', #10118, #1025, #14943 ) ;
#13254 = CARTESIAN_POINT ( 'NONE',  ( -33.14240505666059988, 8.120575443056504028, 17.15924262193565397 ) ) ;
#13255 = VECTOR ( 'NONE', #8799, 1000.000000000000227 ) ;
#13256 = EDGE_CURVE ( 'NONE', #11290, #12569, #8233, .T. ) ;
#13257 = CARTESIAN_POINT ( 'NONE',  ( -11.06429811985332279, -4.540650544146559220, 61.44996607439977510 ) ) ;
#13258 = SHAPE_DEFINITION_REPRESENTATION ( #11040, #10170 ) ;
#13259 = DIRECTION ( 'NONE',  ( 0.9925461516413219831, 0.006378148623808976847, 0.1217023257055283719 ) ) ;
#13260 = LINE ( 'NONE', #4218, #5674 ) ;
#13261 = AXIS2_PLACEMENT_3D ( 'NONE', #7831, #3267, #8065 ) ;
#13262 = DIRECTION ( 'NONE',  ( -0.9885168150181788960, 0.1511109077013150503, -8.829475928589270966E-16 ) ) ;
#13263 = AXIS2_PLACEMENT_3D ( 'NONE', #9648, #9870, #2609 ) ;
#13264 = VERTEX_POINT ( 'NONE', #12688 ) ;
#13265 = ORIENTED_EDGE ( 'NONE', *, *, #5507, .T. ) ;
#13266 = ORIENTED_EDGE ( 'NONE', *, *, #14393, .F. ) ;
#13267 = CIRCLE ( 'NONE', #3230, 9.974999999999999645 ) ;
#13268 = CIRCLE ( 'NONE', #1280, 4.499999999999998224 ) ;
#13269 = DIRECTION ( 'NONE',  ( 0.5975035461963188466, 0.8018662683283437342, 0.000000000000000000 ) ) ;
#13270 = VERTEX_POINT ( 'NONE', #142 ) ;
#13271 = DIRECTION ( 'NONE',  ( 0.3956847857120158740, -0.9183863840214728791, 0.000000000000000000 ) ) ;
#13272 = EDGE_CURVE ( 'NONE', #14077, #5522, #10266, .T. ) ;
#13273 = FACE_OUTER_BOUND ( 'NONE', #2283, .T. ) ;
#13274 = CARTESIAN_POINT ( 'NONE',  ( -23.52886110248590867, -17.73748770914800943, 56.85231026484398598 ) ) ;
#13275 = VECTOR ( 'NONE', #9904, 1000.000000000000000 ) ;
#13276 = VECTOR ( 'NONE', #7114, 1000.000000000000114 ) ;
#13277 = EDGE_CURVE ( 'NONE', #14554, #8561, #2201, .T. ) ;
#13278 = CYLINDRICAL_SURFACE ( 'NONE', #9482, 5.000000000000000000 ) ;
#13280 = CARTESIAN_POINT ( 'NONE',  ( -15.49969986081092088, -13.50737899243822504, 57.00231026484397745 ) ) ;
#13279 = CARTESIAN_POINT ( 'NONE',  ( -14.61203582817000246, -106.9748017008338365, -5.104852750214475599 ) ) ;
#13281 = EDGE_LOOP ( 'NONE', ( #2003, #7519, #14644, #2681 ) ) ;
#13282 = FACE_OUTER_BOUND ( 'NONE', #7983, .T. ) ;
#13283 = ORIENTED_EDGE ( 'NONE', *, *, #2707, .T. ) ;
#13284 = FACE_OUTER_BOUND ( 'NONE', #3565, .T. ) ;
#13285 = ORIENTED_EDGE ( 'NONE', *, *, #2855, .T. ) ;
#13286 = ORIENTED_EDGE ( 'NONE', *, *, #2780, .F. ) ;
#13287 = DIRECTION ( 'NONE',  ( -1.000000000000000000, -1.201369187114119994E-15, -9.616040805000176517E-16 ) ) ;
#13288 = ORIENTED_EDGE ( 'NONE', *, *, #5850, .F. ) ;
#13289 = EDGE_CURVE ( 'NONE', #14240, #7684, #4650, .T. ) ;
#13290 = CIRCLE ( 'NONE', #10586, 2.000000000000001776 ) ;
#13291 = VECTOR ( 'NONE', #4752, 1000.000000000000000 ) ;
#13292 = AXIS2_PLACEMENT_3D ( 'NONE', #11141, #1884, #11363 ) ;
#13293 = EDGE_CURVE ( 'NONE', #3663, #8391, #6850, .T. ) ;
#13294 = DIRECTION ( 'NONE',  ( 0.000000000000000000, -2.220446049250312588E-16, 1.000000000000000000 ) ) ;
#13295 = CARTESIAN_POINT ( 'NONE',  ( -13.16883223745437448, -21.23902216335526916, 56.85231026484400019 ) ) ;
#13296 = EDGE_CURVE ( 'NONE', #12386, #2212, #11731, .T. ) ;
#13297 = CARTESIAN_POINT ( 'NONE',  ( -9.755182731580834599, -21.69540791116318346, 56.55967645960267021 ) ) ;
#13298 = EDGE_CURVE ( 'NONE', #13889, #775, #10865, .T. ) ;
#13299 = CIRCLE ( 'NONE', #585, 9.974999999999999645 ) ;
#13300 = CARTESIAN_POINT ( 'NONE',  ( -15.49969986081100082, -107.0696085497772430, -4.320874558545138022 ) ) ;
#13301 = CARTESIAN_POINT ( 'NONE',  ( -16.26465502354534465, -4.464365468230401923, 57.00231026484397745 ) ) ;
#13302 = ORIENTED_EDGE ( 'NONE', *, *, #1971, .F. ) ;
#13303 = LINE ( 'NONE', #11218, #1896 ) ;
#13304 = DIRECTION ( 'NONE',  ( 1.000000000000000000, 0.000000000000000000, 0.000000000000000000 ) ) ;
#13305 = VERTEX_POINT ( 'NONE', #6993 ) ;
#13306 = CARTESIAN_POINT ( 'NONE',  ( 21.91135930735600468, -25.02476975920917113, 21.62815801113326941 ) ) ;
#13307 = ORIENTED_EDGE ( 'NONE', *, *, #11666, .F. ) ;
#13308 = CARTESIAN_POINT ( 'NONE',  ( -11.90127153857799769, -52.50737899243803497, 11.50231026484396857 ) ) ;
#13309 = EDGE_LOOP ( 'NONE', ( #8563, #3604, #10796, #13868 ) ) ;
#13310 = CARTESIAN_POINT ( 'NONE',  ( -14.95642007119148076, -3.547184613301321399, 54.00231026484397745 ) ) ;
#13311 = COLOUR_RGB ( '', 0.66274510, 0.83137255, 0.94901961) ;
#13312 = CARTESIAN_POINT ( 'NONE',  ( -16.15629313678505952, -110.0846357213627300, -10.93586162601466860 ) ) ;
#13313 = EDGE_CURVE ( 'NONE', #7829, #8731, #10303, .T. ) ;
#13314 = LINE ( 'NONE', #12304, #10675 ) ;
#13315 = AXIS2_PLACEMENT_3D ( 'NONE', #3257, #12594, #10361 ) ;
#13316 = CARTESIAN_POINT ( 'NONE',  ( 15.03585100355005189, -28.72364914449597251, 2.443890032762031872 ) ) ;
#13317 = LINE ( 'NONE', #5119, #9385 ) ;
#13318 = ORIENTED_EDGE ( 'NONE', *, *, #2319, .T. ) ;
#13319 = CARTESIAN_POINT ( 'NONE',  ( -32.89917128247499534, 9.436645346093119002, 31.84501495524920500 ) ) ;
#13320 = DIRECTION ( 'NONE',  ( 8.018662683283438208E-16, -5.975035461963189015E-16, -1.000000000000000000 ) ) ;
#13321 = VECTOR ( 'NONE', #8051, 1000.000000000000000 ) ;
#13322 = ORIENTED_EDGE ( 'NONE', *, *, #2223, .T. ) ;
#13323 = ORIENTED_EDGE ( 'NONE', *, *, #5891, .F. ) ;
#13325 = ORIENTED_EDGE ( 'NONE', *, *, #13682, .F. ) ;
#13324 = CYLINDRICAL_SURFACE ( 'NONE', #4485, 2.500000000000000000 ) ;
#13326 = ORIENTED_EDGE ( 'NONE', *, *, #12628, .F. ) ;
#13327 = EDGE_CURVE ( 'NONE', #259, #14313, #5723, .T. ) ;
#13328 = DIRECTION ( 'NONE',  ( 0.5975035461963189576, 0.8018662683283437342, 0.000000000000000000 ) ) ;
#13329 = PLANE ( 'NONE',  #9000 ) ;
#13330 =( BOUNDED_CURVE ( )  B_SPLINE_CURVE ( 3, ( #14043, #3859, #46, #10668 ),
 .UNSPECIFIED., .F., .F. ) 
 B_SPLINE_CURVE_WITH_KNOTS ( ( 4, 4 ),
 ( -8.881784197001252323E-16, 1.570796326794896114 ),
 .UNSPECIFIED. ) 
 CURVE ( )  GEOMETRIC_REPRESENTATION_ITEM ( )  RATIONAL_B_SPLINE_CURVE ( ( 1.000000000000000000, 0.8047378541243649375, 0.8047378541243649375, 1.000000000000000000 ) ) 
 REPRESENTATION_ITEM ( '' )  );
#13331 = DIRECTION ( 'NONE',  ( -8.018662683283438208E-16, 5.975035461963189015E-16, 1.000000000000000000 ) ) ;
#13332 = VECTOR ( 'NONE', #5818, 1000.000000000000114 ) ;
#13333 = CARTESIAN_POINT ( 'NONE',  ( -9.394734159045251332, -5.558363548092267514, 61.21584039466183924 ) ) ;
#13334 = DIRECTION ( 'NONE',  ( -8.673617379884027583E-16, 1.000000000000000000, 0.000000000000000000 ) ) ;
#13335 = CARTESIAN_POINT ( 'NONE',  ( -1.821162622431179878, -46.50737899243799234, -5.497689735156000346 ) ) ;
#13336 = DIRECTION ( 'NONE',  ( -0.9868311969055004740, -0.1617534816134024167, -6.946583704589977600E-16 ) ) ;
#13337 = CARTESIAN_POINT ( 'NONE',  ( -6.540243082598547808, -14.95284924095401458, 56.85231026484400019 ) ) ;
#13338 = ORIENTED_EDGE ( 'NONE', *, *, #2611, .F. ) ;
#13339 = DIRECTION ( 'NONE',  ( -1.000000000000000000, -1.201369187114119994E-15, -9.616040805000176517E-16 ) ) ;
#13340 = ORIENTED_EDGE ( 'NONE', *, *, #9974, .T. ) ;
#13341 = VERTEX_POINT ( 'NONE', #5853 ) ;
#13342 = EDGE_CURVE ( 'NONE', #13608, #2908, #10383, .T. ) ;
#13343 = ORIENTED_EDGE ( 'NONE', *, *, #11686, .T. ) ;
#13344 = LINE ( 'NONE', #7588, #7547 ) ;
#13345 = CARTESIAN_POINT ( 'NONE',  ( -17.20133171717847631, -6.639650181150215325, 56.85231026484398598 ) ) ;
#13346 = CIRCLE ( 'NONE', #12613, 5.250000000000000888 ) ;
#13347 = AXIS2_PLACEMENT_3D ( 'NONE', #13459, #6549, #753 ) ;
#13348 = DIRECTION ( 'NONE',  ( 0.5975035461963189576, 0.8018662683283437342, 0.000000000000000000 ) ) ;
#13349 = VERTEX_POINT ( 'NONE', #61 ) ;
#13350 = DIRECTION ( 'NONE',  ( 0.000000000000000000, 1.000000000000000000, 1.224646799147350002E-16 ) ) ;
#13351 = CARTESIAN_POINT ( 'NONE',  ( -5.524802968312264362, -13.55273297815671008, 54.00231026484399166 ) ) ;
#13352 = EDGE_LOOP ( 'NONE', ( #360, #4204 ) ) ;
#13353 = VERTEX_POINT ( 'NONE', #10610 ) ;
#13354 = CARTESIAN_POINT ( 'NONE',  ( 2.500300139188996074, -46.50737899243799944, 47.50231026484399877 ) ) ;
#13355 = ADVANCED_FACE ( 'NONE', ( #14975 ), #9389, .F. ) ;
#13356 = DIRECTION ( 'NONE',  ( 0.000000000000000000, 1.369518533665900312E-16, -1.000000000000000000 ) ) ;
#13357 = ORIENTED_EDGE ( 'NONE', *, *, #3431, .F. ) ;
#13358 = DIRECTION ( 'NONE',  ( -8.018662683283438208E-16, 5.975035461963189015E-16, 1.000000000000000000 ) ) ;
#13359 = EDGE_CURVE ( 'NONE', #10020, #3526, #5934, .T. ) ;
#13360 = LINE ( 'NONE', #12208, #5971 ) ;
#13361 = CARTESIAN_POINT ( 'NONE',  ( -14.61203582817000246, -106.7748397497402806, -5.108753790441424414 ) ) ;
#13362 = CARTESIAN_POINT ( 'NONE',  ( -11.00816613584963299, -22.44192803192691343, 56.73235138750358431 ) ) ;
#13363 = DIRECTION ( 'NONE',  ( 0.000000000000000000, 0.000000000000000000, 1.000000000000000000 ) ) ;
#13364 = CARTESIAN_POINT ( 'NONE',  ( -12.84854673063650132, -12.36513540471286454, 56.75231026484397745 ) ) ;
#13365 = ORIENTED_EDGE ( 'NONE', *, *, #5998, .F. ) ;
#13366 = DIRECTION ( 'NONE',  ( 0.000000000000000000, 0.000000000000000000, -1.000000000000000000 ) ) ;
#13367 = AXIS2_PLACEMENT_3D ( 'NONE', #6790, #11472, #996 ) ;
#13368 = DIRECTION ( 'NONE',  ( 0.000000000000000000, 0.1872998510044689147, 0.9823027872370635460 ) ) ;
#13369 = EDGE_LOOP ( 'NONE', ( #9770, #2955, #4810, #5699 ) ) ;
#13370 = ADVANCED_FACE ( 'NONE', ( #3800 ), #1355, .F. ) ;
#13372 = EDGE_CURVE ( 'NONE', #14381, #3567, #13520, .T. ) ;
#13371 = CARTESIAN_POINT ( 'NONE',  ( 21.85920135429435263, -27.00737899243800300, 27.46206422150099868 ) ) ;
#13373 = EDGE_LOOP ( 'NONE', ( #7522, #4885, #5515, #5078 ) ) ;
#13374 = CARTESIAN_POINT ( 'NONE',  ( -16.42437072798637843, -22.03270794722917714, 57.00231026484399166 ) ) ;
#13375 = VERTEX_POINT ( 'NONE', #7152 ) ;
#13376 = CIRCLE ( 'NONE', #9193, 19.00000000000000000 ) ;
#13377 = CARTESIAN_POINT ( 'NONE',  ( -5.499699860811004370, -46.50737899243799944, 42.00231026484399166 ) ) ;
#13378 = PRODUCT_DEFINITION_SHAPE ( 'NONE', 'NONE',  #9473 ) ;
#13379 = EDGE_CURVE ( 'NONE', #5071, #9234, #2581, .T. ) ;
#13380 = AXIS2_PLACEMENT_3D ( 'NONE', #3349, #145, #11754 ) ;
#13381 = CARTESIAN_POINT ( 'NONE',  ( 22.00030013918900096, -27.00737899243800300, 43.21206422150100224 ) ) ;
#13382 = VECTOR ( 'NONE', #12072, 1000.000000000000000 ) ;
#13383 = EDGE_CURVE ( 'NONE', #1146, #1022, #8381, .T. ) ;
#13384 = CARTESIAN_POINT ( 'NONE',  ( -7.607412389351752680, -48.63717025145547979, 18.15312534442707815 ) ) ;
#13385 = CYLINDRICAL_SURFACE ( 'NONE', #13347, 1.750000000000000666 ) ;
#13386 = DIRECTION ( 'NONE',  ( -1.000000000000000078E-15, 1.000000000000000000, 0.000000000000000000 ) ) ;
#13387 = EDGE_LOOP ( 'NONE', ( #13874, #14210, #15, #8971 ) ) ;
#13388 = CARTESIAN_POINT ( 'NONE',  ( -15.49969986081099904, -19.50737899243800300, 24.21206422150100224 ) ) ;
#13389 = DIRECTION ( 'NONE',  ( 0.5975035461963189576, 0.8018662683283437342, 0.000000000000000000 ) ) ;
#13390 = ORIENTED_EDGE ( 'NONE', *, *, #2990, .T. ) ;
#13391 = EDGE_CURVE ( 'NONE', #13854, #8839, #12305, .T. ) ;
#13392 = ORIENTED_EDGE ( 'NONE', *, *, #11099, .F. ) ;
#13394 = ORIENTED_EDGE ( 'NONE', *, *, #159, .F. ) ;
#13393 = CARTESIAN_POINT ( 'NONE',  ( -33.78790396967208665, -40.33206847766481928, -13.23593384171632259 ) ) ;
#13395 = ORIENTED_EDGE ( 'NONE', *, *, #5790, .F. ) ;
#13396 = AXIS2_PLACEMENT_3D ( 'NONE', #7799, #12488, #2002 ) ;
#13397 = CARTESIAN_POINT ( 'NONE',  ( -22.64353467404651354, -6.545608444567307949, 54.00231026484397745 ) ) ;
#13398 = CARTESIAN_POINT ( 'NONE',  ( -18.09969986081100402, -102.4006707610616900, -5.996718795823452020 ) ) ;
#13399 = DIRECTION ( 'NONE',  ( 0.8885476655824671166, 0.4587843131450204393, 4.383711467890819071E-16 ) ) ;
#13400 = CARTESIAN_POINT ( 'NONE',  ( -33.02621722254092873, 8.688004171162605260, 16.87568207617864502 ) ) ;
#13401 = DIRECTION ( 'NONE',  ( 0.000000000000000000, -2.185478394931410082E-16, 1.000000000000000000 ) ) ;
#13402 = PRODUCT_RELATED_PRODUCT_CATEGORY ( 'part', '', ( #7330 ) ) ;
#13403 = CARTESIAN_POINT ( 'NONE',  ( -19.99969986081099904, -13.50737899243800122, 61.71206422150099513 ) ) ;
#13404 = ADVANCED_FACE ( 'NONE', ( #10766 ), #290, .T. ) ;
#13405 = AXIS2_PLACEMENT_3D ( 'NONE', #7565, #12098, #3829 ) ;
#13406 = CARTESIAN_POINT ( 'NONE',  ( -7.499699860810997265, -44.50737899243797813, 46.00231026484399877 ) ) ;
#13407 = VERTEX_POINT ( 'NONE', #11910 ) ;
#13408 = DIRECTION ( 'NONE',  ( 0.000000000000000000, 1.000000000000000000, 1.224646799147350002E-16 ) ) ;
#13409 = ORIENTED_EDGE ( 'NONE', *, *, #1383, .T. ) ;
#13410 = CARTESIAN_POINT ( 'NONE',  ( 0.8003001391889992266, 11.99262100756199878, 16.16206422150100153 ) ) ;
#13412 = ORIENTED_EDGE ( 'NONE', *, *, #14522, .F. ) ;
#13411 = LINE ( 'NONE', #6279, #3989 ) ;
#13413 = VERTEX_POINT ( 'NONE', #11991 ) ;
#13414 = AXIS2_PLACEMENT_3D ( 'NONE', #14633, #4156, #8736 ) ;
#13415 = CARTESIAN_POINT ( 'NONE',  ( -17.86883904694317238, -3.817807045405071431, 54.00231026484397745 ) ) ;
#13416 = DIRECTION ( 'NONE',  ( -8.018662683283439195E-16, 5.975035461963190001E-16, 1.000000000000000000 ) ) ;
#13417 = ORIENTED_EDGE ( 'NONE', *, *, #3080, .T. ) ;
#13418 = CARTESIAN_POINT ( 'NONE',  ( -9.760873592531980947, -5.348549538251076818, 57.00231026484397745 ) ) ;
#13419 = AXIS2_PLACEMENT_3D ( 'NONE', #11891, #10437, #15104 ) ;
#13420 = CARTESIAN_POINT ( 'NONE',  ( -5.966797098401854349, -16.44411015522000241, 56.85231026484400019 ) ) ;
#13421 = DIRECTION ( 'NONE',  ( 0.000000000000000000, -1.000000000000000000, -1.224646799147350002E-16 ) ) ;
#13422 = AXIS2_PLACEMENT_3D ( 'NONE', #13031, #7029, #10720 ) ;
#13423 = EDGE_CURVE ( 'NONE', #5628, #5678, #8384, .T. ) ;
#13424 = EDGE_CURVE ( 'NONE', #1349, #13936, #5029, .T. ) ;
#13426 = CARTESIAN_POINT ( 'NONE',  ( -13.72291223624743139, -3.691898834178109379, 54.00231026484399166 ) ) ;
#13425 = DIRECTION ( 'NONE',  ( -8.018662683283438208E-16, 5.975035461963189015E-16, 1.000000000000000000 ) ) ;
#13427 = CLOSED_SHELL ( 'NONE', ( #2799, #10318, #6421, #14962, #8310, #13952, #9281, #12246, #5689, #14854, #10305, #14213, #3467, #13727, #2163, #14686, #8473, #14506, #12916, #1932, #13641, #4350, #4304, #13563, #11412, #12005, #12294, #3194, #3378, #11292, #5130, #8574, #3495, #12697, #14749, #14314, #6902, #10418, #14127, #1052, #4494, #4818, #12934, #9050, #14984, #1100, #5518, #5043, #1191, #6129, #7483, #2889, #12118, #140, #7561, #2947, #3935, #2742, #9243, #2647, #2651, #6112, #6173, #7659, #6508, #4006, #1784, #2067, #5686, #10811, #14002, #939, #9558, #779, #5619, #11340, #899, #14286, #8866, #7379, #12857 ) ) ;
#13428 = ORIENTED_EDGE ( 'NONE', *, *, #638, .T. ) ;
#13429 = DIRECTION ( 'NONE',  ( 1.054621095516909827E-16, -1.224646799147350002E-16, 1.000000000000000000 ) ) ;
#13430 = CARTESIAN_POINT ( 'NONE',  ( -15.49969986081092088, -13.50737899243822504, 57.00231026484397745 ) ) ;
#13431 = EDGE_LOOP ( 'NONE', ( #14315, #3445, #14778, #14005 ) ) ;
#13432 = ORIENTED_EDGE ( 'NONE', *, *, #6320, .T. ) ;
#13433 = DIRECTION ( 'NONE',  ( 1.000000000000000000, -1.499759782661860071E-32, 1.224646799147350002E-16 ) ) ;
#13434 = CARTESIAN_POINT ( 'NONE',  ( -17.58380395184910228, -52.23561682427189368, 56.94520027470884571 ) ) ;
#13435 = ORIENTED_EDGE ( 'NONE', *, *, #5850, .T. ) ;
#13436 = AXIS2_PLACEMENT_3D ( 'NONE', #11410, #9111, #15006 ) ;
#13437 = VECTOR ( 'NONE', #1502, 1000.000000000000000 ) ;
#13438 = FACE_OUTER_BOUND ( 'NONE', #952, .T. ) ;
#13439 = CARTESIAN_POINT ( 'NONE',  ( -16.41401162527548507, -4.478243707298169340, 56.85231026484398598 ) ) ;
#13440 = CARTESIAN_POINT ( 'NONE',  ( -11.08622897860377776, -4.561882931743227232, 54.00231026484399166 ) ) ;
#13441 = EDGE_CURVE ( 'NONE', #13156, #12480, #8617, .T. ) ;
#13442 = PLANE ( 'NONE',  #3372 ) ;
#13443 = CONICAL_SURFACE ( 'NONE', #10250, 6.250000000000001776, 0.7853981633974461696 ) ;
#13444 = CARTESIAN_POINT ( 'NONE',  ( -15.49969986081099194, -36.50737899243799944, 11.50231026484399699 ) ) ;
#13445 = CARTESIAN_POINT ( 'NONE',  ( -13.26502611401716081, -13.76954925274777075, 51.25231026484399166 ) ) ;
#13446 = ORIENTED_EDGE ( 'NONE', *, *, #8917, .F. ) ;
#13447 = DIRECTION ( 'NONE',  ( -0.4587843131450204948, 0.8885476655824671166, -8.987940462991649850E-16 ) ) ;
#13448 = CARTESIAN_POINT ( 'NONE',  ( -15.61203582816999891, -108.4210244314312916, -5.847664976093792433 ) ) ;
#13449 = ORIENTED_EDGE ( 'NONE', *, *, #6966, .F. ) ;
#13450 = CIRCLE ( 'NONE', #13934, 9.974999999999999645 ) ;
#13451 = CARTESIAN_POINT ( 'NONE',  ( -15.49969986081092088, -13.50737899243822504, 57.00231026484397745 ) ) ;
#13452 = CARTESIAN_POINT ( 'NONE',  ( -7.480766807389218620, -12.55450823271226746, 56.85231026484400019 ) ) ;
#13453 = EDGE_LOOP ( 'NONE', ( #1694, #8634 ) ) ;
#13454 = CARTESIAN_POINT ( 'NONE',  ( -15.49969986081092088, -13.50737899243822504, 56.85231026484398598 ) ) ;
#13455 = CARTESIAN_POINT ( 'NONE',  ( -12.84854673063650132, -12.36513540471286454, 56.75231026484397745 ) ) ;
#13456 = EDGE_CURVE ( 'NONE', #33, #10747, #6159, .T. ) ;
#13457 = DIRECTION ( 'NONE',  ( 5.000000000000000389E-16, -0.4999999999999998890, 0.8660254037844387076 ) ) ;
#13458 = VECTOR ( 'NONE', #11868, 1000.000000000000000 ) ;
#13459 = CARTESIAN_POINT ( 'NONE',  ( -17.61203582817000068, -107.1622034095870077, -6.087689735156001980 ) ) ;
#13460 = CARTESIAN_POINT ( 'NONE',  ( -18.72761429428784297, -5.025526694139714756, 56.85231026484398598 ) ) ;
#13461 = ADVANCED_FACE ( 'NONE', ( #2806 ), #7385, .T. ) ;
#13462 = ORIENTED_EDGE ( 'NONE', *, *, #14813, .T. ) ;
#13463 = CARTESIAN_POINT ( 'NONE',  ( -1.821162622431179878, -46.50737899243799234, -5.497689735156000346 ) ) ;
#13464 = CARTESIAN_POINT ( 'NONE',  ( -33.37394235882850069, 7.183219930803497633, 17.76912582958182085 ) ) ;
#13465 = ORIENTED_EDGE ( 'NONE', *, *, #10761, .T. ) ;
#13467 = ORIENTED_EDGE ( 'NONE', *, *, #11357, .F. ) ;
#13466 = CARTESIAN_POINT ( 'NONE',  ( -35.04849813642518086, -38.38910658708451251, -12.49920242367386791 ) ) ;
#13468 = EDGE_CURVE ( 'NONE', #4184, #7451, #6230, .T. ) ;
#13469 = VERTEX_POINT ( 'NONE', #4955 ) ;
#13470 = VERTEX_POINT ( 'NONE', #14206 ) ;
#13471 = CARTESIAN_POINT ( 'NONE',  ( -3.508527451665001351, -44.77532818486911736, -5.497689735156003010 ) ) ;
#13472 = DIRECTION ( 'NONE',  ( -1.000000000000000078E-15, 0.000000000000000000, 1.000000000000000000 ) ) ;
#13473 = ADVANCED_FACE ( 'NONE', ( #3950 ), #9766, .F. ) ;
#13474 = DIRECTION ( 'NONE',  ( 0.5975035461963189576, 0.8018662683283437342, 0.000000000000000000 ) ) ;
#13475 = EDGE_CURVE ( 'NONE', #12986, #3416, #8613, .T. ) ;
#13476 = CARTESIAN_POINT ( 'NONE',  ( -14.26755283655060680, -21.48817241857114269, 56.85231026484400019 ) ) ;
#13477 = AXIS2_PLACEMENT_3D ( 'NONE', #5376, #11196, #1936 ) ;
#13478 = CYLINDRICAL_SURFACE ( 'NONE', #2622, 19.00000000000000000 ) ;
#13479 = CARTESIAN_POINT ( 'NONE',  ( -15.83606446161809522, -16.37446674635458166, 56.75231026484397745 ) ) ;
#13480 = ORIENTED_EDGE ( 'NONE', *, *, #13847, .F. ) ;
#13481 = PLANE ( 'NONE',  #5901 ) ;
#13482 = ORIENTED_EDGE ( 'NONE', *, *, #3571, .T. ) ;
#13483 = DIRECTION ( 'NONE',  ( -0.9645173894937584258, -0.2640193276336892381, -6.156614753256587028E-16 ) ) ;
#13484 = VERTEX_POINT ( 'NONE', #5170 ) ;
#13485 = VERTEX_POINT ( 'NONE', #14132 ) ;
#13486 = DIRECTION ( 'NONE',  ( 0.000000000000000000, 0.1872998510044689147, 0.9823027872370635460 ) ) ;
#13488 = ORIENTED_EDGE ( 'NONE', *, *, #3047, .T. ) ;
#13487 = CARTESIAN_POINT ( 'NONE',  ( -20.60611791317904107, -19.76323582219775687, 56.85231026484398598 ) ) ;
#13489 = CIRCLE ( 'NONE', #6625, 9.974999999999999645 ) ;
#13490 = CARTESIAN_POINT ( 'NONE',  ( -14.33378105012738502, -9.151149813406526334, -13.27091190697294998 ) ) ;
#13491 = CARTESIAN_POINT ( 'NONE',  ( -22.08930316869620825, -18.17457871440291228, 56.85231026484398598 ) ) ;
#13492 = DIRECTION ( 'NONE',  ( 0.8885476655824650072, 0.4587843131450243805, 4.383711467890778149E-16 ) ) ;
#13493 = ADVANCED_FACE ( 'NONE', ( #3655 ), #8304, .F. ) ;
#13494 = VECTOR ( 'NONE', #991, 1000.000000000000000 ) ;
#13495 = SHAPE_REPRESENTATION ( 'Dial Adjustment Screw', ( #6789 ), #8995 ) ;
#13496 = VECTOR ( 'NONE', #14296, 1000.000000000000000 ) ;
#13497 = AXIS2_PLACEMENT_3D ( 'NONE', #4478, #5763, #11509 ) ;
#13498 = FACE_OUTER_BOUND ( 'NONE', #14207, .T. ) ;
#13499 = VERTEX_POINT ( 'NONE', #11285 ) ;
#13500 = FACE_OUTER_BOUND ( 'NONE', #7763, .T. ) ;
#13501 = EDGE_LOOP ( 'NONE', ( #4891, #10791, #5220, #11365 ) ) ;
#13502 = ORIENTED_EDGE ( 'NONE', *, *, #3796, .F. ) ;
#13503 = LINE ( 'NONE', #3015, #56 ) ;
#13504 = ORIENTED_EDGE ( 'NONE', *, *, #9908, .F. ) ;
#13506 = ADVANCED_FACE ( 'NONE', ( #1726 ), #12363, .F. ) ;
#13505 = LINE ( 'NONE', #506, #10806 ) ;
#13507 = VECTOR ( 'NONE', #14797, 1000.000000000000000 ) ;
#13508 = AXIS2_PLACEMENT_3D ( 'NONE', #1789, #11120, #6292 ) ;
#13509 = CARTESIAN_POINT ( 'NONE',  ( 3.680924773572380904, 6.563493760827302737, 18.28413564240387856 ) ) ;
#13510 = CARTESIAN_POINT ( 'NONE',  ( 4.185908152460800835, 11.99262100756689620, 32.26206422150099939 ) ) ;
#13511 = DIRECTION ( 'NONE',  ( -8.018662683283439195E-16, 5.975035461963190001E-16, 1.000000000000000000 ) ) ;
#13512 = DIRECTION ( 'NONE',  ( 0.000000000000000000, -1.000000000000000000, -1.224646799147350002E-16 ) ) ;
#13513 = CARTESIAN_POINT ( 'NONE',  ( -18.10194853779420399, -23.13696500758646835, 56.85231026484400019 ) ) ;
#13514 = VERTEX_POINT ( 'NONE', #587 ) ;
#13515 = DIRECTION ( 'NONE',  ( 0.000000000000000000, -2.220446049250313081E-16, 1.000000000000000000 ) ) ;
#13516 = FACE_OUTER_BOUND ( 'NONE', #10053, .T. ) ;
#13517 = ORIENTED_EDGE ( 'NONE', *, *, #6887, .T. ) ;
#13518 = DIRECTION ( 'NONE',  ( -8.018662683283438208E-16, 5.975035461963189015E-16, 1.000000000000000000 ) ) ;
#13519 = VECTOR ( 'NONE', #1748, 1000.000000000000000 ) ;
#13520 = CIRCLE ( 'NONE', #10341, 37.50000000000000000 ) ;
#13521 = LINE ( 'NONE', #14741, #4704 ) ;
#13522 = CARTESIAN_POINT ( 'NONE',  ( -17.88573767796789582, -14.53539822139104842, 51.00231026484399166 ) ) ;
#13523 = DIRECTION ( 'NONE',  ( -1.000000000000000000, -3.700743415417187646E-16, 0.000000000000000000 ) ) ;
#13524 = EDGE_LOOP ( 'NONE', ( #7954, #14049, #7705, #1170, #7848, #11128, #3951 ) ) ;
#13525 = CARTESIAN_POINT ( 'NONE',  ( -15.47724068538499154, -13.46270701644446177, 56.85231026484398598 ) ) ;
#13526 = EDGE_CURVE ( 'NONE', #4722, #11072, #8980, .T. ) ;
#13527 = EDGE_CURVE ( 'NONE', #612, #7478, #580, .T. ) ;
#13528 = FACE_OUTER_BOUND ( 'NONE', #12970, .T. ) ;
#13529 = AXIS2_PLACEMENT_3D ( 'NONE', #2829, #7485, #6780 ) ;
#13530 = DIRECTION ( 'NONE',  ( 0.000000000000000000, 1.131341397376178572E-16, -1.000000000000000000 ) ) ;
#13531 = FACE_OUTER_BOUND ( 'NONE', #4467, .T. ) ;
#13532 = LINE ( 'NONE', #7774, #3037 ) ;
#13533 = VERTEX_POINT ( 'NONE', #13513 ) ;
#13534 = CARTESIAN_POINT ( 'NONE',  ( -9.508527451664999575, -46.50737899243799944, -5.497689735156000346 ) ) ;
#13535 = CARTESIAN_POINT ( 'NONE',  ( -7.661016837782100630, -46.08616143870106185, -3.031138187048190158 ) ) ;
#13536 = VECTOR ( 'NONE', #657, 1000.000000000000114 ) ;
#13537 = ORIENTED_EDGE ( 'NONE', *, *, #10648, .F. ) ;
#13539 = EDGE_LOOP ( 'NONE', ( #5252, #1659, #11816, #1284 ) ) ;
#13538 = DIRECTION ( 'NONE',  ( 1.000000000000000000, 0.000000000000000000, 9.688619527525975741E-16 ) ) ;
#13540 = ORIENTED_EDGE ( 'NONE', *, *, #10868, .T. ) ;
#13541 = VECTOR ( 'NONE', #13633, 1000.000000000000114 ) ;
#13542 = EDGE_CURVE ( 'NONE', #10935, #8839, #6378, .T. ) ;
#13543 = CARTESIAN_POINT ( 'NONE',  ( -21.79367780933653620, -21.24601366423100401, 57.00231026484397745 ) ) ;
#13544 = CARTESIAN_POINT ( 'NONE',  ( -7.499699860810998153, -44.50737899243799944, 56.13904046828873362 ) ) ;
#13545 = EDGE_CURVE ( 'NONE', #9803, #14198, #3098, .T. ) ;
#13546 = CARTESIAN_POINT ( 'NONE',  ( -10.08476707729037614, -21.88467736064467672, 56.85231026484400019 ) ) ;
#13547 = LINE ( 'NONE', #13618, #11843 ) ;
#13548 = VECTOR ( 'NONE', #9020, 1000.000000000000000 ) ;
#13549 = DIRECTION ( 'NONE',  ( -8.018662683283438208E-16, 5.975035461963189015E-16, 1.000000000000000000 ) ) ;
#13550 = VECTOR ( 'NONE', #12768, 1000.000000000000000 ) ;
#13551 = CARTESIAN_POINT ( 'NONE',  ( -15.49969986081091022, -13.50737899243823215, 46.00231026484398456 ) ) ;
#13552 = EDGE_CURVE ( 'NONE', #5839, #5768, #7154, .T. ) ;
#13553 = DIRECTION ( 'NONE',  ( -8.018662683283438208E-16, 5.975035461963189015E-16, 1.000000000000000000 ) ) ;
#13554 = CARTESIAN_POINT ( 'NONE',  ( -7.512109644807973829, -44.06143319563968674, 43.96819400509183140 ) ) ;
#13555 = VERTEX_POINT ( 'NONE', #7610 ) ;
#13556 = CARTESIAN_POINT ( 'NONE',  ( 16.19611543458935898, -30.09219076442761676, 44.25382773196126607 ) ) ;
#13557 = ORIENTED_EDGE ( 'NONE', *, *, #7383, .T. ) ;
#13558 = DIRECTION ( 'NONE',  ( 0.000000000000000000, 0.000000000000000000, 1.000000000000000000 ) ) ;
#13559 = EDGE_LOOP ( 'NONE', ( #10306, #11738 ) ) ;
#13560 = ORIENTED_EDGE ( 'NONE', *, *, #7943, .F. ) ;
#13561 = EDGE_CURVE ( 'NONE', #6010, #14217, #14877, .T. ) ;
#13562 = CARTESIAN_POINT ( 'NONE',  ( -9.508527451665001351, -45.50737899243799944, -5.497689735156000346 ) ) ;
#13563 = ADVANCED_FACE ( 'NONE', ( #14732 ), #6456, .T. ) ;
#13565 = ORIENTED_EDGE ( 'NONE', *, *, #3494, .F. ) ;
#13564 = CARTESIAN_POINT ( 'NONE',  ( 2.234407040561845026, 7.699995122702122607, 17.38035637616411222 ) ) ;
#13566 = CARTESIAN_POINT ( 'NONE',  ( -15.49969986081099904, 71.39262100756199914, 24.21206422150100579 ) ) ;
#13567 = MECHANICAL_DESIGN_GEOMETRIC_PRESENTATION_REPRESENTATION (  '', ( #1096 ), #2802 ) ;
#13568 = ADVANCED_FACE ( 'NONE', ( #10051 ), #11065, .F. ) ;
#13569 = LINE ( 'NONE', #13491, #13694 ) ;
#13570 = CARTESIAN_POINT ( 'NONE',  ( 0.8003001391889992266, 11.99262100756199878, 24.16206422150099442 ) ) ;
#13571 = EDGE_CURVE ( 'NONE', #2017, #14153, #6529, .T. ) ;
#13572 = CARTESIAN_POINT ( 'NONE',  ( -17.12834591918736749, -6.622385381944812188, 57.00231026484397745 ) ) ;
#13573 = LINE ( 'NONE', #4160, #12251 ) ;
#13574 = ORIENTED_EDGE ( 'NONE', *, *, #8016, .F. ) ;
#13575 = LINE ( 'NONE', #10112, #6527 ) ;
#13576 = ORIENTED_EDGE ( 'NONE', *, *, #10197, .T. ) ;
#13577 = DIRECTION ( 'NONE',  ( -0.8018662683283436232, 0.5975035461963189576, -9.999999999999998805E-16 ) ) ;
#13578 = ORIENTED_EDGE ( 'NONE', *, *, #2797, .T. ) ;
#13579 = ORIENTED_EDGE ( 'NONE', *, *, #2040, .F. ) ;
#13580 = DIRECTION ( 'NONE',  ( 0.000000000000000000, -1.225619847157526848E-16, 1.000000000000000000 ) ) ;
#13581 = ADVANCED_FACE ( 'NONE', ( #658, #2875 ), #6679, .T. ) ;
#13582 = ORIENTED_EDGE ( 'NONE', *, *, #14300, .F. ) ;
#13583 = CARTESIAN_POINT ( 'NONE',  ( -15.23828507852217129, -36.50737899243799944, 57.00231026484397745 ) ) ;
#13584 = CARTESIAN_POINT ( 'NONE',  ( -12.37415300023346809, -4.034703455804747207, 57.00231026484397745 ) ) ;
#13585 = CARTESIAN_POINT ( 'NONE',  ( -7.499699860810999041, -44.50737899243799944, -17.13441993860073964 ) ) ;
#13586 = CIRCLE ( 'NONE', #13832, 0.2000000000000012046 ) ;
#13587 = LINE ( 'NONE', #13660, #9959 ) ;
#13588 = ADVANCED_FACE ( 'NONE', ( #14804 ), #886, .F. ) ;
#13589 = LINE ( 'NONE', #14580, #7901 ) ;
#13591 = DIRECTION ( 'NONE',  ( 1.000000000000000000, 1.201369187114119994E-15, 9.616040805000176517E-16 ) ) ;
#13590 = PLANE ( 'NONE',  #6661 ) ;
#13592 = ORIENTED_EDGE ( 'NONE', *, *, #6252, .T. ) ;
#13593 = CARTESIAN_POINT ( 'NONE',  ( -7.499699860810999041, -19.50737899243799589, 6.712064221500998684 ) ) ;
#13594 = DIRECTION ( 'NONE',  ( -0.9988970074402867549, 0.04695496274985035828, -8.290375725550441510E-16 ) ) ;
#13595 = ORIENTED_EDGE ( 'NONE', *, *, #3831, .F. ) ;
#13596 = CARTESIAN_POINT ( 'NONE',  ( 2.026817500918900006, 8.688004171162612366, 31.54844636682341275 ) ) ;
#13597 = CARTESIAN_POINT ( 'NONE',  ( 2.500300139188999182, -51.00737899243799944, 52.39987856403599409 ) ) ;
#13598 = AXIS2_PLACEMENT_3D ( 'NONE', #10929, #9707, #233 ) ;
#13599 = CARTESIAN_POINT ( 'NONE',  ( -7.499699860810999041, -19.50737899243799589, 48.00231026484399877 ) ) ;
#13600 = ORIENTED_EDGE ( 'NONE', *, *, #11394, .T. ) ;
#13601 = DIRECTION ( 'NONE',  ( 0.000000000000000000, 0.000000000000000000, -1.000000000000000000 ) ) ;
#13602 = LINE ( 'NONE', #12454, #2445 ) ;
#13603 = DIRECTION ( 'NONE',  ( 1.000000000000000000, 8.224083780703685054E-16, -6.312960948933948519E-16 ) ) ;
#13604 = LINE ( 'NONE', #9150, #3343 ) ;
#13605 = EDGE_CURVE ( 'NONE', #7024, #9434, #8865, .T. ) ;
#13606 = CARTESIAN_POINT ( 'NONE',  ( -15.61203582817000068, -107.1621692949231459, -5.034900018422284518 ) ) ;
#13607 = CARTESIAN_POINT ( 'NONE',  ( -13.09722856071139496, -21.21670818843173478, 57.00231026484399166 ) ) ;
#13608 = VERTEX_POINT ( 'NONE', #14581 ) ;
#13609 = CARTESIAN_POINT ( 'NONE',  ( -32.98605307870397496, 8.906201437969643919, 31.64365951543691935 ) ) ;
#13610 = CARTESIAN_POINT ( 'NONE',  ( -7.510639545435999764, -44.94673998318546637, -3.544435685291067895 ) ) ;
#13611 = STYLED_ITEM ( 'NONE', ( #13076 ), #2616 ) ;
#13612 = VERTEX_POINT ( 'NONE', #4100 ) ;
#13614 = EDGE_LOOP ( 'NONE', ( #12912, #1014, #7027, #15016 ) ) ;
#13613 = CARTESIAN_POINT ( 'NONE',  ( -15.36741682587554969, -22.58172476492607572, 56.85231026484400019 ) ) ;
#13615 = ORIENTED_EDGE ( 'NONE', *, *, #4789, .T. ) ;
#13616 = CARTESIAN_POINT ( 'NONE',  ( -22.42051587769119791, -8.443926053929422082, 56.85231026484398598 ) ) ;
#13617 = CARTESIAN_POINT ( 'NONE',  ( -8.131654986474892155, -16.81240013151894175, 57.00231026484399166 ) ) ;
#13618 = CARTESIAN_POINT ( 'NONE',  ( -16.24959055444668365, -20.54292544936667397, 56.85231026484400019 ) ) ;
#13619 = CIRCLE ( 'NONE', #6510, 2.999999999999999112 ) ;
#13620 = CYLINDRICAL_SURFACE ( 'NONE', #3588, 3.000000000000002665 ) ;
#13621 = ADVANCED_FACE ( 'NONE', ( #8909 ), #13590, .T. ) ;
#13622 = CARTESIAN_POINT ( 'NONE',  ( 0.8003001391889992266, 11.99262100756199878, 24.26206422150100295 ) ) ;
#13623 = AXIS2_PLACEMENT_3D ( 'NONE', #3425, #4354, #1204 ) ;
#13624 = CARTESIAN_POINT ( 'NONE',  ( -6.758527451664999575, -46.50737899243799944, -5.497689735156000346 ) ) ;
#13625 = PLANE ( 'NONE',  #7391 ) ;
#13626 = EDGE_CURVE ( 'NONE', #1039, #13227, #4486, .T. ) ;
#13627 = TOROIDAL_SURFACE ( 'NONE', #3360, 1.600000000000000089, 0.1499999999999999944 ) ;
#13628 = CARTESIAN_POINT ( 'NONE',  ( 16.90549927255504059, -30.26092226866779100, 43.08547782963380968 ) ) ;
#13629 = ORIENTED_EDGE ( 'NONE', *, *, #15020, .T. ) ;
#13631 = ORIENTED_EDGE ( 'NONE', *, *, #3453, .T. ) ;
#13630 = LINE ( 'NONE', #8878, #5210 ) ;
#13632 = CYLINDRICAL_SURFACE ( 'NONE', #13396, 9.974999999999999645 ) ;
#13634 = ORIENTED_EDGE ( 'NONE', *, *, #10566, .F. ) ;
#13633 = DIRECTION ( 'NONE',  ( -0.5491495666976170531, 0.8357240892757724637, -9.396926207859082113E-16 ) ) ;
#13635 = CARTESIAN_POINT ( 'NONE',  ( -10.99969986081100082, -13.50737899243800122, 61.71206422150099513 ) ) ;
#13636 = AXIS2_PLACEMENT_3D ( 'NONE', #2676, #2600, #6024 ) ;
#13637 = CIRCLE ( 'NONE', #7015, 37.50000000000000000 ) ;
#13638 = CIRCLE ( 'NONE', #3625, 5.371426149148541107 ) ;
#13639 = CARTESIAN_POINT ( 'NONE',  ( -15.09158957740191731, -106.8344286703292028, -4.368659857491134169 ) ) ;
#13640 = AXIS2_PLACEMENT_3D ( 'NONE', #6345, #2914, #12171 ) ;
#13641 = ADVANCED_FACE ( 'NONE', ( #9132 ), #7055, .F. ) ;
#13642 = LINE ( 'NONE', #13572, #11507 ) ;
#13643 = DIRECTION ( 'NONE',  ( 0.000000000000000000, -1.000000000000000000, -1.224646799147350002E-16 ) ) ;
#13644 = ADVANCED_FACE ( 'NONE', ( #6751 ), #11733, .T. ) ;
#13645 = ORIENTED_EDGE ( 'NONE', *, *, #8439, .T. ) ;
#13646 = DIRECTION ( 'NONE',  ( 0.000000000000000000, -1.000000000000000000, -1.224646799147350002E-16 ) ) ;
#13647 = VERTEX_POINT ( 'NONE', #2260 ) ;
#13648 = DIRECTION ( 'NONE',  ( -1.000000000000000078E-15, 1.000000000000000000, 0.000000000000000000 ) ) ;
#13649 = ORIENTED_EDGE ( 'NONE', *, *, #11870, .T. ) ;
#13650 = ORIENTED_EDGE ( 'NONE', *, *, #1503, .F. ) ;
#13651 = CARTESIAN_POINT ( 'NONE',  ( -22.54723635769173384, -9.564857042577559199, 56.85231026484398598 ) ) ;
#13652 = DIRECTION ( 'NONE',  ( 1.445602896647339656E-16, 0.000000000000000000, -1.000000000000000000 ) ) ;
#13653 = ORIENTED_EDGE ( 'NONE', *, *, #13153, .F. ) ;
#13654 = ADVANCED_FACE ( 'NONE', ( #13735 ), #4406, .T. ) ;
#13655 = CARTESIAN_POINT ( 'NONE',  ( -10.61847719068383178, -38.14777797243608859, 56.68582056335808517 ) ) ;
#13656 = AXIS2_PLACEMENT_3D ( 'NONE', #2255, #6900, #5536 ) ;
#13657 = FACE_BOUND ( 'NONE', #13785, .T. ) ;
#13658 = CARTESIAN_POINT ( 'NONE',  ( 1.760741030006599317, 10.68321993080349763, 16.26994987741148790 ) ) ;
#13659 = EDGE_CURVE ( 'NONE', #3165, #8545, #9369, .T. ) ;
#13660 = CARTESIAN_POINT ( 'NONE',  ( -16.84408283975263032, -15.31157809617700316, 51.00231026484399166 ) ) ;
#13661 = UNCERTAINTY_MEASURE_WITH_UNIT (LENGTH_MEASURE( 1.000000000000000082E-05 ), #14710, 'distance_accuracy_value', 'NONE');
#13662 = EDGE_CURVE ( 'NONE', #12839, #10153, #9286, .T. ) ;
#13664 = CARTESIAN_POINT ( 'NONE',  ( 5.324488449731577866, 5.776599650193906754, 29.29976833248339574 ) ) ;
#13663 = CARTESIAN_POINT ( 'NONE',  ( -15.49969986081092088, -13.50737899243822504, 56.85231026484398598 ) ) ;
#13665 = VERTEX_POINT ( 'NONE', #3556 ) ;
#13666 = CARTESIAN_POINT ( 'NONE',  ( -5.499699860811000818, -46.50737899243799944, 19.50231026484399877 ) ) ;
#13667 = VECTOR ( 'NONE', #1361, 1000.000000000000000 ) ;
#13668 = FACE_OUTER_BOUND ( 'NONE', #3582, .T. ) ;
#13669 = EDGE_LOOP ( 'NONE', ( #9298, #10490, #782, #2098 ) ) ;
#13670 = AXIS2_PLACEMENT_3D ( 'NONE', #101, #24, #8345 ) ;
#13671 = ORIENTED_EDGE ( 'NONE', *, *, #9627, .T. ) ;
#13672 = CARTESIAN_POINT ( 'NONE',  ( -1.821162622431179878, -46.50737899243799234, -5.497689735156000346 ) ) ;
#13673 = CARTESIAN_POINT ( 'NONE',  ( -22.67768377378909506, -40.96543783778685821, -17.30451537288594110 ) ) ;
#13674 = DIRECTION ( 'NONE',  ( -0.3857661296576155308, -0.9225966037272105291, 2.419218955996680478E-16 ) ) ;
#13675 = CARTESIAN_POINT ( 'NONE',  ( -100.5053766806731090, -107.1622034095863825, -6.087689735156085469 ) ) ;
#13676 = CARTESIAN_POINT ( 'NONE',  ( -15.49969986081099904, 22.99262100756200056, 24.21206422150099868 ) ) ;
#13677 = CIRCLE ( 'NONE', #6080, 2.500000000000002220 ) ;
#13678 = SHAPE_DEFINITION_REPRESENTATION ( #423, #13495 ) ;
#13679 = CARTESIAN_POINT ( 'NONE',  ( -7.638565634192136855, -48.52246210452846498, 20.98308540249201926 ) ) ;
#13680 = DIRECTION ( 'NONE',  ( -8.018662683283438208E-16, 5.975035461963189015E-16, 1.000000000000000000 ) ) ;
#13681 = LINE ( 'NONE', #7841, #7671 ) ;
#13682 = EDGE_CURVE ( 'NONE', #9718, #5071, #11657, .T. ) ;
#13683 = ORIENTED_EDGE ( 'NONE', *, *, #12174, .F. ) ;
#13684 = CARTESIAN_POINT ( 'NONE',  ( -14.93044674059276034, -93.95605536819624604, -0.1564500571729600387 ) ) ;
#13685 = CARTESIAN_POINT ( 'NONE',  ( -7.508516329967514835, -44.90912954173229821, -3.575286200065592279 ) ) ;
#13686 = LINE ( 'NONE', #7846, #8149 ) ;
#13687 = ORIENTED_EDGE ( 'NONE', *, *, #9889, .F. ) ;
#13689 = VERTEX_POINT ( 'NONE', #6904 ) ;
#13688 = DIRECTION ( 'NONE',  ( 1.000000000000000000, 1.000000000000000078E-15, 0.000000000000000000 ) ) ;
#13690 = ORIENTED_EDGE ( 'NONE', *, *, #10584, .F. ) ;
#13691 = DIRECTION ( 'NONE',  ( 8.018662683283438208E-16, -5.975035461963189015E-16, -1.000000000000000000 ) ) ;
#13692 = DIRECTION ( 'NONE',  ( 8.018662683283438208E-16, -5.975035461963189015E-16, -1.000000000000000000 ) ) ;
#13693 = EDGE_CURVE ( 'NONE', #7394, #337, #2412, .T. ) ;
#13694 = VECTOR ( 'NONE', #6358, 1000.000000000000114 ) ;
#13695 = PLANE ( 'NONE',  #6881 ) ;
#13696 = CARTESIAN_POINT ( 'NONE',  ( -7.796313671854394833, -46.67229257320486369, 42.00231026484398456 ) ) ;
#13697 = DIRECTION ( 'NONE',  ( -3.632077277826439854E-16, 1.000000000000000000, 0.000000000000000000 ) ) ;
#13698 = CYLINDRICAL_SURFACE ( 'NONE', #8457, 3.249999999999999556 ) ;
#13699 = DIRECTION ( 'NONE',  ( 0.7953815700667019595, 0.6061090314442014737, 2.756373558169989438E-16 ) ) ;
#13700 = DIRECTION ( 'NONE',  ( -0.1960948578651675878, 0.9805849309054466278, -7.431448254773955467E-16 ) ) ;
#13701 = ORIENTED_EDGE ( 'NONE', *, *, #4125, .T. ) ;
#13702 = LINE ( 'NONE', #5434, #10298 ) ;
#13703 = ORIENTED_EDGE ( 'NONE', *, *, #10445, .T. ) ;
#13704 = DIRECTION ( 'NONE',  ( -8.018662683283438208E-16, 5.975035461963189015E-16, 1.000000000000000000 ) ) ;
#13706 = ORIENTED_EDGE ( 'NONE', *, *, #12823, .F. ) ;
#13705 = DIRECTION ( 'NONE',  ( -0.01206535623792160013, -0.9999272109403024578, 5.877852522924710079E-16 ) ) ;
#13707 = ORIENTED_EDGE ( 'NONE', *, *, #6061, .F. ) ;
#13708 = CARTESIAN_POINT ( 'NONE',  ( -15.49969986081099194, -32.00737899243799944, 19.50231026484399166 ) ) ;
#13709 = ORIENTED_EDGE ( 'NONE', *, *, #8537, .T. ) ;
#13710 = DIRECTION ( 'NONE',  ( 1.000000000000000000, 1.000000000000000078E-15, 0.000000000000000000 ) ) ;
#13711 = EDGE_CURVE ( 'NONE', #5900, #8946, #1068, .T. ) ;
#13712 = VECTOR ( 'NONE', #6763, 1000.000000000000000 ) ;
#13713 = FACE_OUTER_BOUND ( 'NONE', #8512, .T. ) ;
#13714 = ORIENTED_EDGE ( 'NONE', *, *, #12063, .F. ) ;
#13715 = FACE_OUTER_BOUND ( 'NONE', #6815, .T. ) ;
#13716 = FACE_OUTER_BOUND ( 'NONE', #14698, .T. ) ;
#13717 = ORIENTED_EDGE ( 'NONE', *, *, #6626, .F. ) ;
#13718 = CARTESIAN_POINT ( 'NONE',  ( 18.52080869893816839, -26.54306194185273426, 39.98729300097398465 ) ) ;
#13719 = ORIENTED_EDGE ( 'NONE', *, *, #8347, .T. ) ;
#13720 = LINE ( 'NONE', #13945, #4566 ) ;
#13721 = ORIENTED_EDGE ( 'NONE', *, *, #5260, .F. ) ;
#13722 = VERTEX_POINT ( 'NONE', #1182 ) ;
#13723 = AXIS2_PLACEMENT_3D ( 'NONE', #3753, #10484, #11555 ) ;
#13724 = DIRECTION ( 'NONE',  ( 8.018662683283438208E-16, -5.975035461963189015E-16, -1.000000000000000000 ) ) ;
#13725 = VERTEX_POINT ( 'NONE', #5540 ) ;
#13726 = CARTESIAN_POINT ( 'NONE',  ( -8.211338606302485132, -41.19849018162404519, 56.28736606044791557 ) ) ;
#13727 = ADVANCED_FACE ( 'NONE', ( #11435 ), #339, .F. ) ;
#13728 = EDGE_CURVE ( 'NONE', #10111, #8833, #2183, .T. ) ;
#13729 = CARTESIAN_POINT ( 'NONE',  ( -25.43486656742121355, -12.61682438329676081, 56.85231026484398598 ) ) ;
#13730 = CONICAL_SURFACE ( 'NONE', #10304, 1.300000000000000488, 0.1221730476396025861 ) ;
#13731 = DIRECTION ( 'NONE',  ( -0.1617534816134024167, 0.9868311969055004740, -7.193398003386505973E-16 ) ) ;
#13732 = AXIS2_PLACEMENT_3D ( 'NONE', #3404, #10436, #12393 ) ;
#13733 = CARTESIAN_POINT ( 'NONE',  ( 15.21039067757261520, -24.94558503991284226, 2.690838063943358449 ) ) ;
#13734 = CARTESIAN_POINT ( 'NONE',  ( -15.49969986081099904, 20.99262100756200056, 32.26206422150099939 ) ) ;
#13736 = CARTESIAN_POINT ( 'NONE',  ( -17.72867398697626129, -22.30470383268854562, 57.00231026484399166 ) ) ;
#13735 = FACE_OUTER_BOUND ( 'NONE', #10138, .T. ) ;
#13737 = ORIENTED_EDGE ( 'NONE', *, *, #1688, .T. ) ;
#13738 = CARTESIAN_POINT ( 'NONE',  ( -15.49969986081099904, -27.00737899243800300, -5.497689735156002122 ) ) ;
#13739 = DIRECTION ( 'NONE',  ( -1.000000000000000000, 1.499759782661860071E-32, -1.224646799147350002E-16 ) ) ;
#13740 = ORIENTED_EDGE ( 'NONE', *, *, #6459, .F. ) ;
#13741 = CARTESIAN_POINT ( 'NONE',  ( 22.00030013918900096, -27.00737899243800300, 5.212064221501000461 ) ) ;
#13742 = AXIS2_PLACEMENT_3D ( 'NONE', #9214, #9141, #11371 ) ;
#13743 = CARTESIAN_POINT ( 'NONE',  ( -22.29394651601237953, -40.27574555278066981, -17.37736014901681969 ) ) ;
#13744 = CIRCLE ( 'NONE', #9834, 9.974999999999999645 ) ;
#13745 = DIRECTION ( 'NONE',  ( 0.000000000000000000, 0.1872998510044759646, 0.9823027872370621028 ) ) ;
#13746 = ORIENTED_EDGE ( 'NONE', *, *, #10282, .T. ) ;
#13747 = FACE_OUTER_BOUND ( 'NONE', #4945, .T. ) ;
#13748 = CIRCLE ( 'NONE', #13030, 5.250000000000000888 ) ;
#13749 = AXIS2_PLACEMENT_3D ( 'NONE', #9576, #9424, #5894 ) ;
#13750 = EDGE_CURVE ( 'NONE', #9567, #234, #12802, .T. ) ;
#13751 = EDGE_CURVE ( 'NONE', #13829, #5017, #3258, .T. ) ;
#13752 = CARTESIAN_POINT ( 'NONE',  ( -5.499699860811004370, -46.50737899243799944, 44.50231026484399877 ) ) ;
#13753 = CARTESIAN_POINT ( 'NONE',  ( -7.594860258898399330, -10.18326093375929631, 57.00231026484399166 ) ) ;
#13754 = CARTESIAN_POINT ( 'NONE',  ( -21.17290370923395670, -9.280041403099277275, 56.85231026484398598 ) ) ;
#13755 = LINE ( 'NONE', #7552, #9638 ) ;
#13756 = ORIENTED_EDGE ( 'NONE', *, *, #1220, .F. ) ;
#13757 = CARTESIAN_POINT ( 'NONE',  ( -11.40937861856655999, -90.81835191606845115, -2.015739043402887898 ) ) ;
#13758 = CARTESIAN_POINT ( 'NONE',  ( -7.509222570460704738, -44.92217572422880778, -3.564520568178003668 ) ) ;
#13759 = LINE ( 'NONE', #3282, #7663 ) ;
#13760 = ORIENTED_EDGE ( 'NONE', *, *, #10648, .T. ) ;
#13761 = PLANE ( 'NONE',  #2048 ) ;
#13762 = ORIENTED_EDGE ( 'NONE', *, *, #4779, .F. ) ;
#13763 = CARTESIAN_POINT ( 'NONE',  ( -21.89842656004739396, -7.071732433740530510, 56.85231026484398598 ) ) ;
#13764 = CARTESIAN_POINT ( 'NONE',  ( -8.567699421354552314, -48.50933269009345139, 56.35625304898181298 ) ) ;
#13765 = EDGE_CURVE ( 'NONE', #8005, #3663, #12595, .T. ) ;
#13766 = ADVANCED_FACE ( 'NONE', ( #10285 ), #14956, .T. ) ;
#13767 = VECTOR ( 'NONE', #3861, 1000.000000000000114 ) ;
#13768 = VECTOR ( 'NONE', #13784, 999.9999999999998863 ) ;
#13769 = ADVANCED_FACE ( 'NONE', ( #10515 ), #1037, .T. ) ;
#13771 = VECTOR ( 'NONE', #812, 1000.000000000000000 ) ;
#13770 = DIRECTION ( 'NONE',  ( 0.000000000000000000, 9.130123557772668334E-17, -1.000000000000000000 ) ) ;
#13772 = CARTESIAN_POINT ( 'NONE',  ( -8.826344180179512833, -48.91964147717249034, 43.82441874199299292 ) ) ;
#13773 = DIRECTION ( 'NONE',  ( 0.000000000000000000, 1.000000000000000000, 1.224646799147350002E-16 ) ) ;
#13774 = DIRECTION ( 'NONE',  ( 8.018662683283438208E-16, -5.975035461963189015E-16, -1.000000000000000000 ) ) ;
#13775 = PRODUCT_RELATED_PRODUCT_CATEGORY ( 'part', '', ( #10923 ) ) ;
#13776 = FACE_OUTER_BOUND ( 'NONE', #8671, .T. ) ;
#13777 = EDGE_CURVE ( 'NONE', #11236, #11735, #10012, .T. ) ;
#13778 = VECTOR ( 'NONE', #4430, 1000.000000000000000 ) ;
#13779 = DIRECTION ( 'NONE',  ( 0.9988970074402866439, -0.04695496274985035134, 8.290375725550441510E-16 ) ) ;
#13780 = ORIENTED_EDGE ( 'NONE', *, *, #6770, .F. ) ;
#13781 = CARTESIAN_POINT ( 'NONE',  ( 18.44249865551014622, -28.13424414313808697, 40.15532763027508167 ) ) ;
#13782 = ORIENTED_EDGE ( 'NONE', *, *, #7342, .T. ) ;
#13783 = CARTESIAN_POINT ( 'NONE',  ( -15.49969986081099371, -26.50737899243800300, 56.85231026484400019 ) ) ;
#13785 = EDGE_LOOP ( 'NONE', ( #1124, #4301, #1007, #9641 ) ) ;
#13784 = DIRECTION ( 'NONE',  ( 0.6334982226805337957, -0.7737441449604673949, 9.702957262759957177E-16 ) ) ;
#13786 = ORIENTED_EDGE ( 'NONE', *, *, #13847, .T. ) ;
#13787 = CARTESIAN_POINT ( 'NONE',  ( -12.58343141761905670, -12.25091104594033098, 57.00231026484397745 ) ) ;
#13788 = ORIENTED_EDGE ( 'NONE', *, *, #5026, .T. ) ;
#13789 = VECTOR ( 'NONE', #2130, 1000.000000000000000 ) ;
#13790 = CARTESIAN_POINT ( 'NONE',  ( -16.49725497239786520, -3.582384846377123733, 56.85231026484398598 ) ) ;
#13791 = VECTOR ( 'NONE', #6327, 1000.000000000000000 ) ;
#13792 = FACE_OUTER_BOUND ( 'NONE', #12711, .T. ) ;
#13793 = ORIENTED_EDGE ( 'NONE', *, *, #13682, .T. ) ;
#13794 = EDGE_CURVE ( 'NONE', #3050, #3447, #8790, .T. ) ;
#13795 = CARTESIAN_POINT ( 'NONE',  ( -23.39591611362797963, -45.81830490939771039, -17.15696593335874454 ) ) ;
#13796 = EDGE_LOOP ( 'NONE', ( #4753, #7933, #1129, #6949 ) ) ;
#13797 = CARTESIAN_POINT ( 'NONE',  ( 15.62447441151310557, -24.37627644466446952, 45.13040448977423580 ) ) ;
#13798 = ORIENTED_EDGE ( 'NONE', *, *, #1720, .T. ) ;
#13799 = PLANE ( 'NONE',  #7491 ) ;
#13800 = ORIENTED_EDGE ( 'NONE', *, *, #8124, .F. ) ;
#13801 = VERTEX_POINT ( 'NONE', #13471 ) ;
#13802 = CARTESIAN_POINT ( 'NONE',  ( 7.200737182676100190, 4.873818854045000037, 20.51204286552489009 ) ) ;
#13803 = ORIENTED_EDGE ( 'NONE', *, *, #14486, .T. ) ;
#13804 = CARTESIAN_POINT ( 'NONE',  ( -8.706569105308981094, -40.27405685900905752, 56.38218252410854348 ) ) ;
#13805 = ADVANCED_FACE ( 'NONE', ( #6710 ), #12552, .F. ) ;
#13806 = CARTESIAN_POINT ( 'NONE',  ( -18.72761429428784297, -5.025526694139714756, 56.85231026484398598 ) ) ;
#13807 = CARTESIAN_POINT ( 'NONE',  ( -10.60715604080722940, -90.60733076827288812, -7.714789323137090093 ) ) ;
#13808 = VECTOR ( 'NONE', #2464, 1000.000000000000000 ) ;
#13809 = DIRECTION ( 'NONE',  ( 8.018662683283438208E-16, -5.975035461963189015E-16, -1.000000000000000000 ) ) ;
#13810 = EDGE_CURVE ( 'NONE', #6515, #11225, #4364, .T. ) ;
#13812 = CARTESIAN_POINT ( 'NONE',  ( -12.98295438134161195, -5.834228258119843247, 57.00231026484397745 ) ) ;
#13811 = DIRECTION ( 'NONE',  ( -0.3204693369899910826, -0.9472588896649086765, 3.090169943749478258E-16 ) ) ;
#13813 = ORIENTED_EDGE ( 'NONE', *, *, #11972, .F. ) ;
#13814 = CARTESIAN_POINT ( 'NONE',  ( -15.49969986081099727, -52.50737899243799944, 2.502310264843994769 ) ) ;
#13815 = CARTESIAN_POINT ( 'NONE',  ( -15.49969986081099904, 4.873818854045000037, 24.21206422150099868 ) ) ;
#13816 = EDGE_LOOP ( 'NONE', ( #11630, #8309, #5419, #396 ) ) ;
#13817 = ORIENTED_EDGE ( 'NONE', *, *, #14251, .T. ) ;
#13818 = CARTESIAN_POINT ( 'NONE',  ( 4.185908152463202470, 11.99262100756819827, 16.16206422150100153 ) ) ;
#13819 = EDGE_CURVE ( 'NONE', #9794, #7829, #2980, .T. ) ;
#13820 = DIRECTION ( 'NONE',  ( 0.000000000000000000, -1.000000000000000000, -1.224646799147350002E-16 ) ) ;
#13821 = PLANE ( 'NONE',  #7424 ) ;
#13822 = ORIENTED_EDGE ( 'NONE', *, *, #3102, .F. ) ;
#13823 = DIRECTION ( 'NONE',  ( 0.000000000000000000, 1.000000000000000000, 1.224646799147350002E-16 ) ) ;
#13824 = DIRECTION ( 'NONE',  ( 9.804908406240741039E-16, -0.05233595624294555548, -0.9986295347545738332 ) ) ;
#13825 = CARTESIAN_POINT ( 'NONE',  ( -20.64795620320353109, -18.36032465801230273, 56.85231026484398598 ) ) ;
#13826 = PLANE ( 'NONE',  #8692 ) ;
#13827 = EDGE_CURVE ( 'NONE', #10974, #5139, #14687, .T. ) ;
#13828 = CARTESIAN_POINT ( 'NONE',  ( -32.76014075162859740, 10.68321993080349763, 32.15417856559049881 ) ) ;
#13829 = VERTEX_POINT ( 'NONE', #13546 ) ;
#13830 = CARTESIAN_POINT ( 'NONE',  ( -14.26921869364951867, -92.83203452458182880, -0.2586353043396797391 ) ) ;
#13831 = ADVANCED_FACE ( 'NONE', ( #689 ), #2068, .F. ) ;
#13832 = AXIS2_PLACEMENT_3D ( 'NONE', #5488, #9001, #10144 ) ;
#13833 = LINE ( 'NONE', #13983, #2133 ) ;
#13834 = DIRECTION ( 'NONE',  ( 0.000000000000000000, 0.000000000000000000, -1.000000000000000000 ) ) ;
#13835 = EDGE_CURVE ( 'NONE', #9099, #4294, #13268, .T. ) ;
#13836 = LINE ( 'NONE', #14623, #9253 ) ;
#13837 = ORIENTED_EDGE ( 'NONE', *, *, #7592, .T. ) ;
#13838 = PLANE ( 'NONE',  #14748 ) ;
#13839 = VERTEX_POINT ( 'NONE', #13617 ) ;
#13840 = FACE_OUTER_BOUND ( 'NONE', #11497, .T. ) ;
#13841 = CARTESIAN_POINT ( 'NONE',  ( -15.09158957740191731, -107.1622034095870077, -6.087689735156000204 ) ) ;
#13842 = EDGE_CURVE ( 'NONE', #5903, #1553, #6562, .T. ) ;
#13843 = CARTESIAN_POINT ( 'NONE',  ( -18.09969986081092230, -100.8057294739168839, -7.021413858388602769 ) ) ;
#13844 = CARTESIAN_POINT ( 'NONE',  ( -5.831322665684755435, -10.89379466358441384, 60.44451731831637886 ) ) ;
#13845 = VECTOR ( 'NONE', #5454, 1000.000000000000000 ) ;
#13846 = CARTESIAN_POINT ( 'NONE',  ( 0.8003001391889992266, 3.992621007561997892, 24.21206422150099868 ) ) ;
#13847 = EDGE_CURVE ( 'NONE', #8177, #5325, #12473, .T. ) ;
#13848 = ADVANCED_FACE ( 'NONE', ( #845 ), #5424, .F. ) ;
#13849 = CARTESIAN_POINT ( 'NONE',  ( -15.49969986081086226, -13.50737899243826767, -13.99768973515600301 ) ) ;
#13850 = FACE_OUTER_BOUND ( 'NONE', #9915, .T. ) ;
#13851 = ORIENTED_EDGE ( 'NONE', *, *, #558, .T. ) ;
#13852 = CARTESIAN_POINT ( 'NONE',  ( 17.35529208743007601, -30.13086992362137551, 42.29099036764831965 ) ) ;
#13853 = AXIS2_PLACEMENT_3D ( 'NONE', #8171, #8400, #8248 ) ;
#13854 = VERTEX_POINT ( 'NONE', #9015 ) ;
#13856 = ORIENTED_EDGE ( 'NONE', *, *, #2144, .F. ) ;
#13855 = CARTESIAN_POINT ( 'NONE',  ( -21.60465186766506918, -5.558554322211025855, 61.21584607775863418 ) ) ;
#13857 = ORIENTED_EDGE ( 'NONE', *, *, #9594, .F. ) ;
#13858 = ORIENTED_EDGE ( 'NONE', *, *, #2608, .T. ) ;
#13859 = AXIS2_PLACEMENT_3D ( 'NONE', #12172, #1690, #11020 ) ;
#13860 = DIRECTION ( 'NONE',  ( 0.000000000000000000, 0.1872998510044759646, 0.9823027872370621028 ) ) ;
#13861 = ADVANCED_FACE ( 'NONE', ( #4208 ), #14836, .F. ) ;
#13862 = CARTESIAN_POINT ( 'NONE',  ( -20.86957454690095304, -106.3702754883801873, -5.355332227506997000 ) ) ;
#13863 =( LENGTH_UNIT ( ) NAMED_UNIT ( * ) SI_UNIT ( .MILLI., .METRE. ) );
#13864 = CIRCLE ( 'NONE', #670, 3.000000000000002665 ) ;
#13865 = AXIS2_PLACEMENT_3D ( 'NONE', #287, #8459, #9909 ) ;
#13866 = ORIENTED_EDGE ( 'NONE', *, *, #936, .F. ) ;
#13867 = CARTESIAN_POINT ( 'NONE',  ( -15.49969986081099371, -52.50737899243799944, -17.99768973515599768 ) ) ;
#13868 = ORIENTED_EDGE ( 'NONE', *, *, #9359, .T. ) ;
#13869 = ADVANCED_FACE ( 'NONE', ( #8864 ), #13695, .F. ) ;
#13870 = CARTESIAN_POINT ( 'NONE',  ( 14.70449519813618977, -26.54667573212512011, 46.43727775870232222 ) ) ;
#13871 = ORIENTED_EDGE ( 'NONE', *, *, #13835, .T. ) ;
#13872 = DIRECTION ( 'NONE',  ( -8.018662683283439195E-16, 5.975035461963190001E-16, 1.000000000000000000 ) ) ;
#13873 = ORIENTED_EDGE ( 'NONE', *, *, #14393, .T. ) ;
#13874 = ORIENTED_EDGE ( 'NONE', *, *, #8645, .T. ) ;
#13875 = FACE_OUTER_BOUND ( 'NONE', #6739, .T. ) ;
#13876 = ORIENTED_EDGE ( 'NONE', *, *, #8917, .T. ) ;
#13877 = VECTOR ( 'NONE', #10235, 1000.000000000000000 ) ;
#13878 = FACE_OUTER_BOUND ( 'NONE', #11875, .T. ) ;
#13879 = VECTOR ( 'NONE', #4363, 1000.000000000000000 ) ;
#13880 = AXIS2_PLACEMENT_3D ( 'NONE', #7263, #7345, #8267 ) ;
#13881 = EDGE_CURVE ( 'NONE', #14240, #11857, #5204, .T. ) ;
#13882 = EDGE_CURVE ( 'NONE', #8949, #4751, #14541, .T. ) ;
#13884 =( NAMED_UNIT ( * ) PLANE_ANGLE_UNIT ( ) SI_UNIT ( $, .RADIAN. ) );
#13883 =( REPRESENTATION_RELATIONSHIP ('NONE','NONE', #2372, #3931 ) REPRESENTATION_RELATIONSHIP_WITH_TRANSFORMATION ( #7995 )SHAPE_REPRESENTATION_RELATIONSHIP( ) );
#13885 = LINE ( 'NONE', #8131, #2931 ) ;
#13886 = CARTESIAN_POINT ( 'NONE',  ( -19.41680297924232335, -22.68108752059492517, 54.00231026484399166 ) ) ;
#13888 = CARTESIAN_POINT ( 'NONE',  ( 5.491220283057865359, 5.696595093589351677, 29.19866481050043561 ) ) ;
#13887 = DIRECTION ( 'NONE',  ( -8.018662683283439195E-16, 5.975035461963190001E-16, 1.000000000000000000 ) ) ;
#13889 = VERTEX_POINT ( 'NONE', #6414 ) ;
#13890 = DIRECTION ( 'NONE',  ( 0.000000000000000000, 9.130123557772668334E-17, -1.000000000000000000 ) ) ;
#13891 = CARTESIAN_POINT ( 'NONE',  ( -19.85590761163705409, -14.67339121653544964, -13.03410041670467301 ) ) ;
#13892 = ORIENTED_EDGE ( 'NONE', *, *, #267, .F. ) ;
#13893 = ORIENTED_EDGE ( 'NONE', *, *, #3136, .F. ) ;
#13894 = DIRECTION ( 'NONE',  ( 0.9868311969055004740, 0.1617534816134024167, 6.946583704589977600E-16 ) ) ;
#13895 = CARTESIAN_POINT ( 'NONE',  ( -15.19690733689918538, -23.47778227853769550, 56.85231026484400019 ) ) ;
#13896 = CARTESIAN_POINT ( 'NONE',  ( -20.64795620320353109, -18.36032465801230273, 56.85231026484398598 ) ) ;
#13897 = ORIENTED_EDGE ( 'NONE', *, *, #13137, .T. ) ;
#13898 = DIRECTION ( 'NONE',  ( 0.000000000000000000, 0.1872998510044759646, 0.9823027872370621028 ) ) ;
#13899 = AXIS2_PLACEMENT_3D ( 'NONE', #13570, #4005, #6359 ) ;
#13900 = ADVANCED_FACE ( 'NONE', ( #9936 ), #14612, .T. ) ;
#13901 = CARTESIAN_POINT ( 'NONE',  ( -21.05979293892203330, -6.334749421441233430, 56.85231026484398598 ) ) ;
#13902 = CARTESIAN_POINT ( 'NONE',  ( -22.70913108387521007, -17.14542124616560770, 56.85231026484398598 ) ) ;
#13903 = AXIS2_PLACEMENT_3D ( 'NONE', #7077, #2662, #13075 ) ;
#13904 = AXIS2_PLACEMENT_3D ( 'NONE', #7192, #11869, #10726 ) ;
#13905 = LINE ( 'NONE', #4498, #6474 ) ;
#13906 = CARTESIAN_POINT ( 'NONE',  ( -15.49969986081099904, -2.007378992438000331, 24.21206422150099513 ) ) ;
#13907 = ORIENTED_EDGE ( 'NONE', *, *, #14845, .F. ) ;
#13908 = PLANE ( 'NONE',  #8972 ) ;
#13909 = CARTESIAN_POINT ( 'NONE',  ( -34.68032449512179483, 6.563493760861876858, 30.13999280063012520 ) ) ;
#13910 = CARTESIAN_POINT ( 'NONE',  ( -18.09969986081099336, -109.4641865893815407, -10.25678343939419968 ) ) ;
#13911 = AXIS2_PLACEMENT_3D ( 'NONE', #3910, #5274, #10875 ) ;
#13912 = DIRECTION ( 'NONE',  ( 0.5975035461963188466, 0.8018662683283437342, 0.000000000000000000 ) ) ;
#13913 = VERTEX_POINT ( 'NONE', #5647 ) ;
#13914 = ORIENTED_EDGE ( 'NONE', *, *, #12435, .T. ) ;
#13915 = DIRECTION ( 'NONE',  ( 0.000000000000000000, 1.224646799147350002E-16, -1.000000000000000000 ) ) ;
#13916 = LINE ( 'NONE', #3433, #9224 ) ;
#13917 = AXIS2_PLACEMENT_3D ( 'NONE', #417, #11033, #2848 ) ;
#13918 = AXIS2_PLACEMENT_3D ( 'NONE', #13381, #4042, #12148 ) ;
#13919 = ADVANCED_FACE ( 'NONE', ( #6787, #2294 ), #4740, .T. ) ;
#13920 = DIRECTION ( 'NONE',  ( 0.000000000000000000, 1.131341397376178572E-16, -1.000000000000000000 ) ) ;
#13921 = FACE_OUTER_BOUND ( 'NONE', #8182, .T. ) ;
#13922 = EDGE_CURVE ( 'NONE', #6446, #12986, #4663, .T. ) ;
#13923 = DIRECTION ( 'NONE',  ( 0.5975035461963189576, 0.8018662683283437342, 0.000000000000000000 ) ) ;
#13924 = DIRECTION ( 'NONE',  ( -1.000000000000000000, 0.000000000000000000, 0.000000000000000000 ) ) ;
#13925 = CARTESIAN_POINT ( 'NONE',  ( -5.966797098401851684, -16.44411015522000596, 54.00231026484400587 ) ) ;
#13926 = LINE ( 'NONE', #11475, #80 ) ;
#13927 = ORIENTED_EDGE ( 'NONE', *, *, #11228, .T. ) ;
#13928 = DIRECTION ( 'NONE',  ( -8.018662683283439195E-16, 5.975035461963190001E-16, 1.000000000000000000 ) ) ;
#13929 = EDGE_LOOP ( 'NONE', ( #4573, #1359, #14328, #9480, #2063, #13933, #13615 ) ) ;
#13930 = DIRECTION ( 'NONE',  ( 0.9966498018049937402, -0.08178736187251965661, 8.480480961564258050E-16 ) ) ;
#13932 = ORIENTED_EDGE ( 'NONE', *, *, #2230, .T. ) ;
#13931 = CARTESIAN_POINT ( 'NONE',  ( -20.79173795306330774, -5.016115743661099913, 61.33778859824581531 ) ) ;
#13933 = ORIENTED_EDGE ( 'NONE', *, *, #8714, .T. ) ;
#13934 = AXIS2_PLACEMENT_3D ( 'NONE', #3627, #6131, #10741 ) ;
#13935 = DIRECTION ( 'NONE',  ( -0.5975035461963190686, -0.8018662683283436232, -2.958228394578794270E-31 ) ) ;
#13936 = VERTEX_POINT ( 'NONE', #9091 ) ;
#13937 = DIRECTION ( 'NONE',  ( 0.000000000000000000, 0.1872998510044983078, 0.9823027872370578839 ) ) ;
#13938 = EDGE_CURVE ( 'NONE', #3375, #6778, #4515, .T. ) ;
#13939 = EDGE_CURVE ( 'NONE', #12240, #1569, #3436, .T. ) ;
#13940 = PLANE ( 'NONE',  #5982 ) ;
#13941 = DIRECTION ( 'NONE',  ( -8.018662683283438208E-16, 5.975035461963189015E-16, 1.000000000000000000 ) ) ;
#13942 = VERTEX_POINT ( 'NONE', #3361 ) ;
#13943 = CARTESIAN_POINT ( 'NONE',  ( -14.33039451911155382, -17.86275798826623173, -13.27081260207403268 ) ) ;
#13944 = VERTEX_POINT ( 'NONE', #5726 ) ;
#13945 = CARTESIAN_POINT ( 'NONE',  ( -25.43486656742120999, -12.61682438329676259, 54.00231026484397745 ) ) ;
#13946 = EDGE_LOOP ( 'NONE', ( #11384, #6869, #796, #8141 ) ) ;
#13947 = VERTEX_POINT ( 'NONE', #10395 ) ;
#13948 = FACE_OUTER_BOUND ( 'NONE', #2607, .T. ) ;
#13949 = CARTESIAN_POINT ( 'NONE',  ( -20.60611791317904107, -19.76323582219775687, 56.85231026484398598 ) ) ;
#13950 = ORIENTED_EDGE ( 'NONE', *, *, #4702, .T. ) ;
#13951 = CARTESIAN_POINT ( 'NONE',  ( -7.499849062438288527, -12.40572695854698360, 56.85231026484400019 ) ) ;
#13952 = ADVANCED_FACE ( 'NONE', ( #4588 ), #543, .T. ) ;
#13953 = CARTESIAN_POINT ( 'NONE',  ( -15.49969986081099016, -27.00737899243800300, 27.50231026484399877 ) ) ;
#13954 = CARTESIAN_POINT ( 'NONE',  ( 3.243537350856608548, 11.48902252479464181, 16.16206422150199629 ) ) ;
#13955 = VECTOR ( 'NONE', #2553, 1000.000000000000000 ) ;
#13956 = PLANE ( 'NONE',  #3514 ) ;
#13958 = DIRECTION ( 'NONE',  ( 0.000000000000000000, 0.000000000000000000, 1.000000000000000000 ) ) ;
#13957 = CARTESIAN_POINT ( 'NONE',  ( -15.49969986081099904, 10.68321993080349586, 43.21206422150100224 ) ) ;
#13959 = ORIENTED_EDGE ( 'NONE', *, *, #11309, .T. ) ;
#13960 = FACE_OUTER_BOUND ( 'NONE', #1282, .T. ) ;
#13961 = CARTESIAN_POINT ( 'NONE',  ( -5.499699860811003482, -46.50737899243799944, 41.50231026484399166 ) ) ;
#13962 = ORIENTED_EDGE ( 'NONE', *, *, #3666, .F. ) ;
#13963 = ORIENTED_EDGE ( 'NONE', *, *, #6340, .T. ) ;
#13964 = DIRECTION ( 'NONE',  ( 0.000000000000000000, 0.000000000000000000, 1.000000000000000000 ) ) ;
#13965 = ADVANCED_FACE ( 'NONE', ( #8085 ), #11470, .F. ) ;
#13966 = DIRECTION ( 'NONE',  ( -0.02283895005205794151, 0.9997391571607663341, -6.156614753256579139E-16 ) ) ;
#13967 = VERTEX_POINT ( 'NONE', #5798 ) ;
#13968 = CARTESIAN_POINT ( 'NONE',  ( -15.61203582816999891, -106.7406604375499626, -7.297873098422156701 ) ) ;
#13969 = ORIENTED_EDGE ( 'NONE', *, *, #12518, .T. ) ;
#13970 = DIRECTION ( 'NONE',  ( 0.000000000000000000, -9.130123557772668334E-17, 1.000000000000000000 ) ) ;
#13971 = APPLICATION_CONTEXT ( 'automotive_design' ) ;
#13972 = AXIS2_PLACEMENT_3D ( 'NONE', #3062, #10253, #14996 ) ;
#13973 = LINE ( 'NONE', #8150, #8038 ) ;
#13974 = CONTEXT_DEPENDENT_SHAPE_REPRESENTATION ( #12409, #6392 ) ;
#13975 = DIRECTION ( 'NONE',  ( -0.8599296884906633132, 0.5104125104778984845, -9.945218953682734920E-16 ) ) ;
#13976 = DIRECTION ( 'NONE',  ( 1.054621095516909827E-16, -1.224646799147350002E-16, 1.000000000000000000 ) ) ;
#13977 = CARTESIAN_POINT ( 'NONE',  ( -34.24293707247814211, 11.48902252479439134, 32.26206422149999753 ) ) ;
#13978 = AXIS2_PLACEMENT_3D ( 'NONE', #279, #11898, #10602 ) ;
#13979 = ORIENTED_EDGE ( 'NONE', *, *, #1407, .F. ) ;
#13980 = CARTESIAN_POINT ( 'NONE',  ( -13.15284510314214295, -91.74749311801966201, -0.6644210899480663679 ) ) ;
#13981 = AXIS2_PLACEMENT_3D ( 'NONE', #2868, #9973, #3738 ) ;
#13982 =( BOUNDED_CURVE ( )  B_SPLINE_CURVE ( 3, ( #7806, #12493, #6663, #11346 ),
 .UNSPECIFIED., .F., .F. ) 
 B_SPLINE_CURVE_WITH_KNOTS ( ( 4, 4 ),
 ( 5.060245233341797544, 5.259239931080632147 ),
 .UNSPECIFIED. ) 
 CURVE ( )  GEOMETRIC_REPRESENTATION_ITEM ( )  RATIONAL_B_SPLINE_CURVE ( ( 1.000000000000000000, 0.9967028139718016044, 0.9967028139718016044, 1.000000000000000000 ) ) 
 REPRESENTATION_ITEM ( '' )  );
#13983 = CARTESIAN_POINT ( 'NONE',  ( -9.499699860810959962, -67.00737899243799234, -5.497689735155993240 ) ) ;
#13984 = DIRECTION ( 'NONE',  ( 0.5975035461963188466, 0.8018662683283437342, 0.000000000000000000 ) ) ;
#13985 = VECTOR ( 'NONE', #8472, 1000.000000000000000 ) ;
#13986 = EDGE_CURVE ( 'NONE', #9646, #8988, #11618, .T. ) ;
#13987 = AXIS2_PLACEMENT_3D ( 'NONE', #2514, #11764, #2594 ) ;
#13988 = CARTESIAN_POINT ( 'NONE',  ( -15.49969986081099904, -19.50737899243800300, 24.21206422150100224 ) ) ;
#13989 = ORIENTED_EDGE ( 'NONE', *, *, #1650, .T. ) ;
#13990 = CARTESIAN_POINT ( 'NONE',  ( -15.31527533914055539, -21.58027268651140673, 56.85231026484400019 ) ) ;
#13991 = ORIENTED_EDGE ( 'NONE', *, *, #7676, .F. ) ;
#13992 = LINE ( 'NONE', #3664, #7859 ) ;
#13993 = DIRECTION ( 'NONE',  ( 8.018662683283438208E-16, -5.975035461963189015E-16, -1.000000000000000000 ) ) ;
#13994 = DIRECTION ( 'NONE',  ( 0.000000000000000000, -1.000000000000000000, -1.224646799147350002E-16 ) ) ;
#13995 = SURFACE_STYLE_FILL_AREA ( #1368 ) ;
#13996 = VECTOR ( 'NONE', #6743, 999.9999999999998863 ) ;
#13997 = VECTOR ( 'NONE', #3768, 1000.000000000000114 ) ;
#13998 = CARTESIAN_POINT ( 'NONE',  ( -17.58300953724144122, -11.95501924286632267, 51.00231026484399166 ) ) ;
#13999 = DIRECTION ( 'NONE',  ( 0.5975035461963189576, 0.8018662683283437342, 0.000000000000000000 ) ) ;
#14000 = DIRECTION ( 'NONE',  ( 0.9983330752162417054, 0.05771543059946734194, 7.660444431189781397E-16 ) ) ;
#14001 = CARTESIAN_POINT ( 'NONE',  ( -31.13003983167857669, -27.07585217469821259, 58.39162460182396330 ) ) ;
#14002 = ADVANCED_FACE ( 'NONE', ( #994 ), #5570, .T. ) ;
#14003 = ORIENTED_EDGE ( 'NONE', *, *, #378, .F. ) ;
#14004 = DIRECTION ( 'NONE',  ( -0.7350174335289139105, 0.6780482080269578660, -9.945218953682732947E-16 ) ) ;
#14005 = ORIENTED_EDGE ( 'NONE', *, *, #13986, .F. ) ;
#14007 = VERTEX_POINT ( 'NONE', #11692 ) ;
#14006 = CARTESIAN_POINT ( 'NONE',  ( -16.15343032139029233, -3.507358680200116208, 61.71206438550458984 ) ) ;
#14008 = ORIENTED_EDGE ( 'NONE', *, *, #14237, .T. ) ;
#14009 = AXIS2_PLACEMENT_3D ( 'NONE', #3600, #7023, #13025 ) ;
#14010 = ADVANCED_FACE ( 'NONE', ( #3511 ), #14914, .F. ) ;
#14011 = CARTESIAN_POINT ( 'NONE',  ( -15.49969986081099904, 0.9926210075619987805, 24.21206422150099868 ) ) ;
#14012 = VERTEX_POINT ( 'NONE', #3291 ) ;
#14013 = LINE ( 'NONE', #3686, #1935 ) ;
#14014 = CARTESIAN_POINT ( 'NONE',  ( -9.031792552787408113, -10.63903015472410374, 57.00231026484399166 ) ) ;
#14015 = CARTESIAN_POINT ( 'NONE',  ( -8.569834614884436874, -19.36726104528708703, 56.85231026484400019 ) ) ;
#14016 = DIRECTION ( 'NONE',  ( 0.000000000000000000, 0.000000000000000000, 1.000000000000000000 ) ) ;
#14017 = CARTESIAN_POINT ( 'NONE',  ( -11.68798435751175369, -21.74340199640734994, 56.85231026484400019 ) ) ;
#14018 = AXIS2_PLACEMENT_3D ( 'NONE', #10538, #8469, #71 ) ;
#14019 = DIRECTION ( 'NONE',  ( 0.5975035461963189576, 0.8018662683283437342, 0.000000000000000000 ) ) ;
#14020 = CARTESIAN_POINT ( 'NONE',  ( -23.24172680504385369, -46.58969747883803336, -17.18995143628628952 ) ) ;
#14021 = EDGE_CURVE ( 'NONE', #11608, #2388, #6153, .T. ) ;
#14022 = EDGE_LOOP ( 'NONE', ( #1306, #3727, #13288, #11127 ) ) ;
#14023 = CARTESIAN_POINT ( 'NONE',  ( 3.154275669408413307, -39.53260173292035518, -13.02893167591090773 ) ) ;
#14024 = EDGE_CURVE ( 'NONE', #6873, #7651, #6861, .T. ) ;
#14025 = EDGE_LOOP ( 'NONE', ( #8417, #6820, #10810, #3465 ) ) ;
#14026 = CARTESIAN_POINT ( 'NONE',  ( -16.32407967933980686, -20.53418644068968746, 56.85231026484400019 ) ) ;
#14027 = ORIENTED_EDGE ( 'NONE', *, *, #14429, .F. ) ;
#14028 = ORIENTED_EDGE ( 'NONE', *, *, #980, .F. ) ;
#14029 = LINE ( 'NONE', #3546, #6152 ) ;
#14030 = EDGE_CURVE ( 'NONE', #7744, #7558, #12626, .T. ) ;
#14031 = CARTESIAN_POINT ( 'NONE',  ( -15.54961651457173488, -13.51026476396819831, 56.85231026484398598 ) ) ;
#14032 = VERTEX_POINT ( 'NONE', #10544 ) ;
#14033 = DIRECTION ( 'NONE',  ( 8.018662683283438208E-16, -5.975035461963189015E-16, -1.000000000000000000 ) ) ;
#14034 = VECTOR ( 'NONE', #4489, 1000.000000000000000 ) ;
#14035 = EDGE_CURVE ( 'NONE', #9929, #2365, #14068, .T. ) ;
#14036 = DIRECTION ( 'NONE',  ( -8.018662683283438208E-16, 5.975035461963189015E-16, 1.000000000000000000 ) ) ;
#14037 = DIRECTION ( 'NONE',  ( -1.000000000000000000, 0.000000000000000000, 0.000000000000000000 ) ) ;
#14038 = CARTESIAN_POINT ( 'NONE',  ( -7.694327897266501459, -46.24447382526680173, 21.98901576030363358 ) ) ;
#14039 = CIRCLE ( 'NONE', #6453, 15.62500000000000355 ) ;
#14041 = CARTESIAN_POINT ( 'NONE',  ( -13.92794721577312878, -5.586467200048621073, 56.85231026484398598 ) ) ;
#14040 = DIRECTION ( 'NONE',  ( 0.000000000000000000, 0.4999999999999993339, 0.8660254037844390407 ) ) ;
#14042 = VERTEX_POINT ( 'NONE', #8246 ) ;
#14043 = CARTESIAN_POINT ( 'NONE',  ( -15.16333526000374832, -10.64029123852186487, 51.25231026484399166 ) ) ;
#14044 = EDGE_CURVE ( 'NONE', #374, #415, #12938, .T. ) ;
#14045 = CARTESIAN_POINT ( 'NONE',  ( -21.67659902633305791, -21.33978230808610022, 54.00231026484399166 ) ) ;
#14046 = ORIENTED_EDGE ( 'NONE', *, *, #7928, .T. ) ;
#14047 = ORIENTED_EDGE ( 'NONE', *, *, #6157, .F. ) ;
#14048 = CARTESIAN_POINT ( 'NONE',  ( -7.902754534677060683, -18.47202114588016642, 56.85231026484400019 ) ) ;
#14049 = ORIENTED_EDGE ( 'NONE', *, *, #5143, .T. ) ;
#14050 = LINE ( 'NONE', #6000, #4509 ) ;
#14051 = ORIENTED_EDGE ( 'NONE', *, *, #283, .T. ) ;
#14052 = VECTOR ( 'NONE', #6038, 1000.000000000000000 ) ;
#14053 = DIRECTION ( 'NONE',  ( -1.000000000000000000, -1.201369187114119994E-15, -9.616040805000176517E-16 ) ) ;
#14054 = EDGE_CURVE ( 'NONE', #13179, #505, #10624, .T. ) ;
#14055 = CARTESIAN_POINT ( 'NONE',  ( -19.62128088291994388, -20.45131122700032833, 57.00231026484397745 ) ) ;
#14056 = CARTESIAN_POINT ( 'NONE',  ( -23.49969986081099904, -44.50737899243799944, -5.497689735156002122 ) ) ;
#14057 = EDGE_LOOP ( 'NONE', ( #8528, #11307, #5660, #13176 ) ) ;
#14058 = CARTESIAN_POINT ( 'NONE',  ( -9.299228256956212135, -8.333850033420862502, 56.85231026484398598 ) ) ;
#14059 = FACE_OUTER_BOUND ( 'NONE', #3202, .T. ) ;
#14060 = EDGE_LOOP ( 'NONE', ( #1397, #6208, #6145, #2246, #9048, #9735, #12926 ) ) ;
#14061 = CARTESIAN_POINT ( 'NONE',  ( -15.49969986081099904, 71.39262100756199914, 24.21206422150100579 ) ) ;
#14062 = ORIENTED_EDGE ( 'NONE', *, *, #866, .F. ) ;
#14063 = CARTESIAN_POINT ( 'NONE',  ( -12.84854673063649599, -12.36513540471286809, 51.25231026484399166 ) ) ;
#14064 = ORIENTED_EDGE ( 'NONE', *, *, #4819, .F. ) ;
#14065 = DIRECTION ( 'NONE',  ( -8.018662683283439195E-16, 5.975035461963190001E-16, 1.000000000000000000 ) ) ;
#14066 = DIRECTION ( 'NONE',  ( -0.5000000000000004441, 0.8660254037844384856, 1.060575238724907408E-16 ) ) ;
#14067 = DIRECTION ( 'NONE',  ( -0.5975035461963189576, -0.8018662683283438453, 9.860761315262649757E-32 ) ) ;
#14068 = LINE ( 'NONE', #8013, #3971 ) ;
#14069 = ADVANCED_FACE ( 'NONE', ( #154, #2820 ), #9550, .F. ) ;
#14070 = CARTESIAN_POINT ( 'NONE',  ( -7.499699860810999041, -19.50737899243799589, 60.84879442494580104 ) ) ;
#14071 =( BOUNDED_CURVE ( )  B_SPLINE_CURVE ( 3, ( #13444, #733, #9840, #11064 ),
 .UNSPECIFIED., .F., .F. ) 
 B_SPLINE_CURVE_WITH_KNOTS ( ( 4, 4 ),
 ( 3.141592653589792672, 4.712388980384689674 ),
 .UNSPECIFIED. ) 
 CURVE ( )  GEOMETRIC_REPRESENTATION_ITEM ( )  RATIONAL_B_SPLINE_CURVE ( ( 1.000000000000000000, 0.8047378541243649375, 0.8047378541243649375, 1.000000000000000000 ) ) 
 REPRESENTATION_ITEM ( '' )  );
#14072 = CIRCLE ( 'NONE', #7468, 19.00000000000000000 ) ;
#14073 = DIRECTION ( 'NONE',  ( 1.000000000000000000, 9.973326722932540411E-16, 9.491043554366112247E-16 ) ) ;
#14074 = CARTESIAN_POINT ( 'NONE',  ( -7.844836682715700782, -47.42038978965683782, -7.826127288787263936 ) ) ;
#14075 = CARTESIAN_POINT ( 'NONE',  ( -7.886584594865190034, -46.96511696614950182, -7.955427708867500058 ) ) ;
#14076 = CARTESIAN_POINT ( 'NONE',  ( -15.49969986081086226, -13.50737899243826767, -13.99768973515600301 ) ) ;
#14077 = VERTEX_POINT ( 'NONE', #1520 ) ;
#14078 = DIRECTION ( 'NONE',  ( 1.000000000000000000, 1.201369187114119994E-15, 9.616040805000176517E-16 ) ) ;
#14079 = VERTEX_POINT ( 'NONE', #6243 ) ;
#14081 = ORIENTED_EDGE ( 'NONE', *, *, #5905, .T. ) ;
#14080 = CARTESIAN_POINT ( 'NONE',  ( 13.85920135429429934, -27.00737899243800300, 5.212064221501000461 ) ) ;
#14082 = ORIENTED_EDGE ( 'NONE', *, *, #9952, .T. ) ;
#14083 = DIRECTION ( 'NONE',  ( 0.5975035461963188466, 0.8018662683283437342, 0.000000000000000000 ) ) ;
#14084 = ORIENTED_EDGE ( 'NONE', *, *, #8456, .T. ) ;
#14085 = VECTOR ( 'NONE', #11174, 999.9999999999998863 ) ;
#14086 = LINE ( 'NONE', #13115, #5352 ) ;
#14087 = DIRECTION ( 'NONE',  ( 8.018662683283438208E-16, -5.975035461963189015E-16, -1.000000000000000000 ) ) ;
#14088 = EDGE_CURVE ( 'NONE', #10261, #12780, #1289, .T. ) ;
#14089 = DIRECTION ( 'NONE',  ( 0.000000000000000000, 1.850371707708594316E-16, -1.000000000000000000 ) ) ;
#14090 = DIRECTION ( 'NONE',  ( 1.000000000000000000, 0.000000000000000000, 0.000000000000000000 ) ) ;
#14091 = CARTESIAN_POINT ( 'NONE',  ( -16.57334897777262483, -22.01522992987520766, 57.00231026484399166 ) ) ;
#14092 = AXIS2_PLACEMENT_3D ( 'NONE', #9018, #5650, #2145 ) ;
#14093 = CYLINDRICAL_SURFACE ( 'NONE', #2064, 5.371426149148541107 ) ;
#14094 = B_SPLINE_CURVE_WITH_KNOTS ( 'NONE', 3,
 ( #1028, #10354, #15023, #3399, #6897, #11579, #10429, #15096, #4621, #12819, #2330, #804, #3549, #2406, #10659, #3779, #2555, #37 ),
 .UNSPECIFIED., .F., .F.,
 ( 4, 2, 2, 2, 1, 1, 2, 2, 2, 4 ),
 ( 0.000000000000000000, 0.2500000000000217604, 0.3750000000000327516, 0.4375000000000378031, 0.4687500000000399125, 0.4843750000000400791, 0.4921875000000398015, 0.5000000000000394129, 0.7500000000000197620, 1.000000000000000000 ),
 .UNSPECIFIED. ) ;
#14095 = DIRECTION ( 'NONE',  ( 1.000000000000000000, 1.201369187114119994E-15, 9.616040805000176517E-16 ) ) ;
#14096 = ORIENTED_EDGE ( 'NONE', *, *, #13765, .T. ) ;
#14097 = CARTESIAN_POINT ( 'NONE',  ( -12.75469031341037685, -17.08519519190822322, -13.18812972638144743 ) ) ;
#14098 = ORIENTED_EDGE ( 'NONE', *, *, #749, .F. ) ;
#14099 = EDGE_LOOP ( 'NONE', ( #1624, #1978, #1885, #4601 ) ) ;
#14100 = CIRCLE ( 'NONE', #8717, 2.500000000000000444 ) ;
#14101 = EDGE_LOOP ( 'NONE', ( #1641, #3841, #5003, #12180, #14426, #14816, #7877, #9371, #9177, #9714, #1677, #143, #2564, #12523, #5918, #14134, #13323, #8197, #5616, #7219, #4986, #8449, #5999 ) ) ;
#14102 = CARTESIAN_POINT ( 'NONE',  ( 5.055282432709286233, -37.64246294776327062, 50.86739471227122067 ) ) ;
#14103 = ORIENTED_EDGE ( 'NONE', *, *, #2030, .T. ) ;
#14104 = LINE ( 'NONE', #9588, #10069 ) ;
#14105 = CIRCLE ( 'NONE', #9208, 2.000000000000001776 ) ;
#14106 = EDGE_CURVE ( 'NONE', #276, #1815, #11848, .T. ) ;
#14107 = FACE_OUTER_BOUND ( 'NONE', #10556, .T. ) ;
#14108 = CARTESIAN_POINT ( 'NONE',  ( -16.58746603607634640, -23.42289157363888208, 57.00231026484399166 ) ) ;
#14109 = EDGE_CURVE ( 'NONE', #9733, #3638, #228, .T. ) ;
#14110 = CARTESIAN_POINT ( 'NONE',  ( -15.09158957740191553, -107.4618831711941169, -7.659374194735306673 ) ) ;
#14112 = CARTESIAN_POINT ( 'NONE',  ( -37.04494295528539993, 12.99262100756199878, 32.26206422150099939 ) ) ;
#14111 = CARTESIAN_POINT ( 'NONE',  ( -7.654737080345056732, -48.45581950336406862, -3.931260860926701461 ) ) ;
#14113 = CARTESIAN_POINT ( 'NONE',  ( -12.51218212982926836, -9.498047650796548780, -13.49768973515600301 ) ) ;
#14114 = B_SPLINE_CURVE_WITH_KNOTS ( 'NONE', 3,
 ( #138, #9452, #14126, #209, #6155, #367, #3649, #9685 ),
 .UNSPECIFIED., .F., .F.,
 ( 4, 2, 2, 4 ),
 ( 0.000000000000000000, 0.2500000000000007216, 0.5000000000000014433, 1.000000000000000000 ),
 .UNSPECIFIED. ) ;
#14115 = AXIS2_PLACEMENT_3D ( 'NONE', #13666, #815, #3331 ) ;
#14116 = DIRECTION ( 'NONE',  ( 0.8719950447285823580, 0.4895147004624046394, 4.067366430758000189E-16 ) ) ;
#14117 = ORIENTED_EDGE ( 'NONE', *, *, #3326, .T. ) ;
#14118 = ADVANCED_FACE ( 'NONE', ( #9780 ), #13163, .F. ) ;
#14119 = VERTEX_POINT ( 'NONE', #14222 ) ;
#14120 = CARTESIAN_POINT ( 'NONE',  ( 21.94825106416211824, -29.59105673714036300, 22.22908312652625540 ) ) ;
#14121 = AXIS2_PLACEMENT_3D ( 'NONE', #14011, #12870, #9260 ) ;
#14122 = CARTESIAN_POINT ( 'NONE',  ( -33.49969986081099904, -42.00737899243800655, -13.39525803434800011 ) ) ;
#14123 = VERTEX_POINT ( 'NONE', #10924 ) ;
#14124 = EDGE_CURVE ( 'NONE', #11072, #6628, #14444, .T. ) ;
#14125 = EDGE_CURVE ( 'NONE', #10705, #12498, #6413, .T. ) ;
#14126 = CARTESIAN_POINT ( 'NONE',  ( 7.492258075141476681, 4.011311318234621837, 24.89656457396599265 ) ) ;
#14127 = ADVANCED_FACE ( 'NONE', ( #1445, #5948 ), #7168, .F. ) ;
#14128 = AXIS2_PLACEMENT_3D ( 'NONE', #10164, #13553, #12400 ) ;
#14129 = CARTESIAN_POINT ( 'NONE',  ( -20.19618812003464470, -21.27295997720514720, 56.85231026484398598 ) ) ;
#14130 = CIRCLE ( 'NONE', #455, 2.499999999999998668 ) ;
#14131 = CARTESIAN_POINT ( 'NONE',  ( -7.494898247900367849, -44.62174188576448586, 17.84928634147309268 ) ) ;
#14132 = CARTESIAN_POINT ( 'NONE',  ( -21.60512016940287694, -5.619130273271677467, 56.85231026484398598 ) ) ;
#14133 = B_SPLINE_CURVE_WITH_KNOTS ( 'NONE', 3,
 ( #8609, #583, #2801, #12131, #2949, #5246, #6305, #10984, #6523, #5165, #9838, #14505 ),
 .UNSPECIFIED., .F., .F.,
 ( 4, 2, 2, 2, 2, 4 ),
 ( 0.004466813839283045873, 0.005050776363214819209, 0.005634738887146591678, 0.006218701411078365014, 0.006510682673044269030, 0.006802663935010173045 ),
 .UNSPECIFIED. ) ;
#14134 = ORIENTED_EDGE ( 'NONE', *, *, #7206, .F. ) ;
#14135 = LINE ( 'NONE', #10533, #3599 ) ;
#14136 = CARTESIAN_POINT ( 'NONE',  ( -35.89253646483789595, 5.983413651708109349, 29.54306818915388533 ) ) ;
#14137 = ORIENTED_EDGE ( 'NONE', *, *, #6229, .F. ) ;
#14138 = VECTOR ( 'NONE', #5227, 999.9999999999998863 ) ;
#14139 = FACE_OUTER_BOUND ( 'NONE', #2229, .T. ) ;
#14140 = EDGE_LOOP ( 'NONE', ( #4979, #343, #5088, #8057 ) ) ;
#14141 = AXIS2_PLACEMENT_3D ( 'NONE', #1888, #6534, #2954 ) ;
#14142 = FACE_OUTER_BOUND ( 'NONE', #12408, .T. ) ;
#14143 = ORIENTED_EDGE ( 'NONE', *, *, #10543, .F. ) ;
#14144 = DIRECTION ( 'NONE',  ( 1.000000000000000000, 1.201369187114119994E-15, 9.616040805000176517E-16 ) ) ;
#14145 = DIRECTION ( 'NONE',  ( 1.000000000000000000, 1.201369187114119994E-15, 9.616040805000176517E-16 ) ) ;
#14146 = DIRECTION ( 'NONE',  ( 8.018662683283438208E-16, -5.975035461963189015E-16, -1.000000000000000000 ) ) ;
#14147 = CARTESIAN_POINT ( 'NONE',  ( -15.49969986081091733, -13.50737899243822682, 54.00231026484399166 ) ) ;
#14148 = EDGE_CURVE ( 'NONE', #700, #9278, #794, .T. ) ;
#14150 = AXIS2_PLACEMENT_3D ( 'NONE', #5640, #10312, #13912 ) ;
#14149 = FILL_AREA_STYLE_COLOUR ( '', #124 ) ;
#14151 = CARTESIAN_POINT ( 'NONE',  ( -15.49969986081086226, -13.50737899243826767, -13.99768973515600301 ) ) ;
#14152 = CARTESIAN_POINT ( 'NONE',  ( 18.17353442779068473, -29.10076824620873026, 7.707990019632498857 ) ) ;
#14153 = VERTEX_POINT ( 'NONE', #10779 ) ;
#14154 = CYLINDRICAL_SURFACE ( 'NONE', #14352, 8.000000000000000000 ) ;
#14155 = CARTESIAN_POINT ( 'NONE',  ( -35.19389501775997786, -38.25609885807658372, 51.41451777256275335 ) ) ;
#14156 = DIRECTION ( 'NONE',  ( -8.018662683283438208E-16, 5.975035461963189015E-16, 1.000000000000000000 ) ) ;
#14157 = ORIENTED_EDGE ( 'NONE', *, *, #11079, .T. ) ;
#14158 = CARTESIAN_POINT ( 'NONE',  ( -6.405625242116718354, -17.60596799715946759, 57.00231026484399166 ) ) ;
#14159 = UNCERTAINTY_MEASURE_WITH_UNIT (LENGTH_MEASURE( 1.000000000000000082E-05 ), #9265, 'distance_accuracy_value', 'NONE');
#14160 = VECTOR ( 'NONE', #1783, 1000.000000000000000 ) ;
#14161 = ORIENTED_EDGE ( 'NONE', *, *, #12650, .F. ) ;
#14163 = ORIENTED_EDGE ( 'NONE', *, *, #14611, .F. ) ;
#14162 = CARTESIAN_POINT ( 'NONE',  ( 0.8003001391889992266, 20.99262100756200056, 24.21206422150099868 ) ) ;
#14164 = VERTEX_POINT ( 'NONE', #6017 ) ;
#14165 = VECTOR ( 'NONE', #10299, 1000.000000000000114 ) ;
#14166 = EDGE_CURVE ( 'NONE', #2405, #4751, #10700, .T. ) ;
#14167 = DIRECTION ( 'NONE',  ( 8.018662683283438208E-16, -5.975035461963189015E-16, -1.000000000000000000 ) ) ;
#14168 = ORIENTED_EDGE ( 'NONE', *, *, #11594, .T. ) ;
#14169 = CARTESIAN_POINT ( 'NONE',  ( 4.185908152460800835, 11.99262100756689620, 32.26206422150099939 ) ) ;
#14170 = CARTESIAN_POINT ( 'NONE',  ( -13.09722856071139496, -21.21670818843173478, 56.85231026484400019 ) ) ;
#14171 = CARTESIAN_POINT ( 'NONE',  ( -6.309378268457432881, -9.629413800598410234, 54.00231026484399166 ) ) ;
#14172 = CARTESIAN_POINT ( 'NONE',  ( -19.07412756035248336, -10.75766711226809669, -13.11755961025760442 ) ) ;
#14173 = AXIS2_PLACEMENT_3D ( 'NONE', #2181, #2027, #11506 ) ;
#14174 = DIRECTION ( 'NONE',  ( -1.000000000000000000, -1.927249326158839857E-15, 7.070501591499359300E-17 ) ) ;
#14175 = CARTESIAN_POINT ( 'NONE',  ( 5.196266986419307621, -37.55864118711512845, -11.77116662607953046 ) ) ;
#14176 = AXIS2_PLACEMENT_3D ( 'NONE', #7729, #711, #9815 ) ;
#14177 = ORIENTED_EDGE ( 'NONE', *, *, #9802, .F. ) ;
#14178 = ORIENTED_EDGE ( 'NONE', *, *, #4551, .F. ) ;
#14179 = EDGE_LOOP ( 'NONE', ( #2475, #224, #3639, #6225 ) ) ;
#14180 = EDGE_CURVE ( 'NONE', #11896, #14475, #11041, .T. ) ;
#14181 = CARTESIAN_POINT ( 'NONE',  ( -10.85342163307452523, -20.71489927548028476, 57.00231026484399166 ) ) ;
#14182 = ORIENTED_EDGE ( 'NONE', *, *, #5549, .T. ) ;
#14183 = DIRECTION ( 'NONE',  ( 0.000000000000000000, 1.131341397376178572E-16, -1.000000000000000000 ) ) ;
#14184 = DIRECTION ( 'NONE',  ( -1.000000000000000000, -1.201369187114119994E-15, -9.616040805000176517E-16 ) ) ;
#14185 = CARTESIAN_POINT ( 'NONE',  ( -15.49969986081099904, 64.39262100756199914, 24.21206422150100224 ) ) ;
#14186 = VECTOR ( 'NONE', #8266, 1000.000000000000114 ) ;
#14187 = DIRECTION ( 'NONE',  ( 0.000000000000000000, -1.000000000000000000, -1.224646799147350002E-16 ) ) ;
#14189 = DIRECTION ( 'NONE',  ( 0.000000000000000000, 1.508455196501571429E-16, -1.000000000000000000 ) ) ;
#14188 = CARTESIAN_POINT ( 'NONE',  ( -7.501950027729723303, -44.50597529135383468, 20.99749114769749880 ) ) ;
#14190 = ORIENTED_EDGE ( 'NONE', *, *, #10982, .T. ) ;
#14191 = CARTESIAN_POINT ( 'NONE',  ( -17.47506273705024071, -21.33739760717825718, 57.00231026484399166 ) ) ;
#14192 = CARTESIAN_POINT ( 'NONE',  ( -19.41680297924232690, -22.68108752059492517, 56.85231026484400019 ) ) ;
#14193 = VERTEX_POINT ( 'NONE', #4970 ) ;
#14194 = ORIENTED_EDGE ( 'NONE', *, *, #13750, .F. ) ;
#14195 = DIRECTION ( 'NONE',  ( 0.6251242923673516749, 0.7805252200231699300, 3.489949670249872777E-17 ) ) ;
#14196 = EDGE_CURVE ( 'NONE', #8556, #4184, #4951, .T. ) ;
#14197 = CARTESIAN_POINT ( 'NONE',  ( -17.71337442941458207, -109.0839711032716934, -1.566993409155049255 ) ) ;
#14198 = VERTEX_POINT ( 'NONE', #9702 ) ;
#14199 = DIRECTION ( 'NONE',  ( 0.9966498018049937402, -0.08178736187251965661, 8.480480961564258050E-16 ) ) ;
#14200 = EDGE_CURVE ( 'NONE', #2938, #10535, #14377, .T. ) ;
#14201 = DIRECTION ( 'NONE',  ( 0.5975035461963189576, 0.8018662683283437342, 0.000000000000000000 ) ) ;
#14202 = CIRCLE ( 'NONE', #11747, 0.2000000000000012046 ) ;
#14203 = FACE_OUTER_BOUND ( 'NONE', #14926, .T. ) ;
#14204 = EDGE_CURVE ( 'NONE', #10009, #11853, #13235, .T. ) ;
#14205 = CARTESIAN_POINT ( 'NONE',  ( -12.51218212982926836, -9.498047650796547003, -13.99768973515600301 ) ) ;
#14206 = CARTESIAN_POINT ( 'NONE',  ( -20.48903913017556633, -19.85700446605285308, 57.00231026484397745 ) ) ;
#14207 = EDGE_LOOP ( 'NONE', ( #7047, #14695, #10887, #127 ) ) ;
#14208 = CARTESIAN_POINT ( 'NONE',  ( -0.3742611254310204694, -27.95036676736704706, 53.90694524323487258 ) ) ;
#14209 = CARTESIAN_POINT ( 'NONE',  ( -7.223083447440863836, -17.23012942000294245, 56.85231026484400019 ) ) ;
#14210 = ORIENTED_EDGE ( 'NONE', *, *, #8868, .T. ) ;
#14211 = ADVANCED_FACE ( 'NONE', ( #457 ), #12082, .T. ) ;
#14213 = ADVANCED_FACE ( 'NONE', ( #10141 ), #10311, .T. ) ;
#14212 = DIRECTION ( 'NONE',  ( -8.018662683283438208E-16, 5.975035461963189015E-16, 1.000000000000000000 ) ) ;
#14214 = DIRECTION ( 'NONE',  ( 0.000000000000000000, -1.225619847157526848E-16, 1.000000000000000000 ) ) ;
#14215 = ORIENTED_EDGE ( 'NONE', *, *, #3515, .T. ) ;
#14216 = CARTESIAN_POINT ( 'NONE',  ( 0.8003001391889992266, 3.992621007561997892, 24.16206422150099442 ) ) ;
#14217 = VERTEX_POINT ( 'NONE', #13455 ) ;
#14218 = AXIS2_PLACEMENT_3D ( 'NONE', #86, #4600, #11779 ) ;
#14219 = ADVANCED_FACE ( 'NONE', ( #523 ), #4266, .F. ) ;
#14220 = CARTESIAN_POINT ( 'NONE',  ( -11.49119621977820671, -37.57910197549196596, 56.78818114396622718 ) ) ;
#14221 = FACE_OUTER_BOUND ( 'NONE', #5198, .T. ) ;
#14222 = CARTESIAN_POINT ( 'NONE',  ( -15.49969986081099194, -110.0146955301539151, -11.10449286955627102 ) ) ;
#14223 = FACE_OUTER_BOUND ( 'NONE', #13796, .T. ) ;
#14224 = EDGE_CURVE ( 'NONE', #12498, #13305, #5183, .T. ) ;
#14225 = CARTESIAN_POINT ( 'NONE',  ( -12.51218212982932165, -9.498047650796509700, 51.00031026484398922 ) ) ;
#14226 = VECTOR ( 'NONE', #1330, 1000.000000000000000 ) ;
#14227 = CIRCLE ( 'NONE', #7619, 4.500000000000000000 ) ;
#14228 = VECTOR ( 'NONE', #10474, 1000.000000000000000 ) ;
#14229 = CARTESIAN_POINT ( 'NONE',  ( -18.61476135779618346, -20.95734656753543845, 57.00231026484397745 ) ) ;
#14230 = ORIENTED_EDGE ( 'NONE', *, *, #10869, .T. ) ;
#14231 = CARTESIAN_POINT ( 'NONE',  ( -11.95839784354461521, -51.68564174154704460, -17.83082277104466939 ) ) ;
#14232 = CARTESIAN_POINT ( 'NONE',  ( -33.73358454970886555, -40.49459960334031905, 52.27083934352044992 ) ) ;
#14233 = PLANE ( 'NONE',  #10084 ) ;
#14234 = ORIENTED_EDGE ( 'NONE', *, *, #7282, .T. ) ;
#14235 = LINE ( 'NONE', #5734, #4199 ) ;
#14236 = EDGE_CURVE ( 'NONE', #11873, #6817, #13602, .T. ) ;
#14237 = EDGE_CURVE ( 'NONE', #6582, #3521, #8698, .T. ) ;
#14238 = EDGE_LOOP ( 'NONE', ( #2732, #4470, #13322, #5105 ) ) ;
#14240 = VERTEX_POINT ( 'NONE', #2888 ) ;
#14239 = CARTESIAN_POINT ( 'NONE',  ( -15.61203582817000068, -106.7748397497402806, -5.108753790441425302 ) ) ;
#14241 = ORIENTED_EDGE ( 'NONE', *, *, #11245, .T. ) ;
#14242 = LINE ( 'NONE', #5965, #7513 ) ;
#14243 = ORIENTED_EDGE ( 'NONE', *, *, #4870, .T. ) ;
#14244 = VECTOR ( 'NONE', #6190, 1000.000000000000000 ) ;
#14245 = AXIS2_PLACEMENT_3D ( 'NONE', #8723, #2991, #8874 ) ;
#14246 = CARTESIAN_POINT ( 'NONE',  ( -18.48721759179245439, -17.51671033407998479, -13.49768973515600301 ) ) ;
#14247 = FACE_OUTER_BOUND ( 'NONE', #10173, .T. ) ;
#14248 = CARTESIAN_POINT ( 'NONE',  ( 16.50882759085405738, -66.53588008523861674, 30.32497911656573208 ) ) ;
#14249 = PRODUCT_DEFINITION ( 'UNKNOWN', '', #9259, #12794 ) ;
#14250 = FACE_OUTER_BOUND ( 'NONE', #9850, .T. ) ;
#14251 = EDGE_CURVE ( 'NONE', #3246, #10391, #5596, .T. ) ;
#14252 = VECTOR ( 'NONE', #10940, 1000.000000000000000 ) ;
#14253 = DIRECTION ( 'NONE',  ( 0.3956847857120158740, -0.9183863840214728791, 0.000000000000000000 ) ) ;
#14254 = CARTESIAN_POINT ( 'NONE',  ( -25.24719169991952583, -11.38911842147176756, 56.85231026484398598 ) ) ;
#14255 = ORIENTED_EDGE ( 'NONE', *, *, #5564, .T. ) ;
#14256 = ORIENTED_EDGE ( 'NONE', *, *, #12346, .T. ) ;
#14257 = VERTEX_POINT ( 'NONE', #12302 ) ;
#14258 = CARTESIAN_POINT ( 'NONE',  ( -6.507973901336479017, -12.27851192488648024, 56.85231026484400019 ) ) ;
#14259 = ORIENTED_EDGE ( 'NONE', *, *, #4232, .F. ) ;
#14260 = CARTESIAN_POINT ( 'NONE',  ( -7.711221940648826489, -11.37542292179617753, 56.85231026484400019 ) ) ;
#14261 = FACE_OUTER_BOUND ( 'NONE', #4924, .T. ) ;
#14262 = VECTOR ( 'NONE', #12299, 1000.000000000000114 ) ;
#14263 = DIRECTION ( 'NONE',  ( 0.5975035461963188466, 0.8018662683283438453, 0.000000000000000000 ) ) ;
#14264 = DIRECTION ( 'NONE',  ( 0.000000000000000000, -0.1872998510044521503, -0.9823027872370667657 ) ) ;
#14265 = VECTOR ( 'NONE', #12135, 999.9999999999998863 ) ;
#14266 = EDGE_CURVE ( 'NONE', #3050, #9211, #5485, .T. ) ;
#14267 = DIRECTION ( 'NONE',  ( 1.000000000000000472E-15, -0.9823027872370664326, 0.1872998510044539822 ) ) ;
#14269 = CARTESIAN_POINT ( 'NONE',  ( -38.24611845019376943, 4.729174316169127756, 27.62997877663899615 ) ) ;
#14268 = CARTESIAN_POINT ( 'NONE',  ( -7.662963790453773072, -48.42200951437354206, -7.105263616372978319 ) ) ;
#14270 = EDGE_LOOP ( 'NONE', ( #10367, #3939, #2001, #10732 ) ) ;
#14271 = DIRECTION ( 'NONE',  ( 0.09252159378508259535, -0.9957106782009863544, 6.691306063588661357E-16 ) ) ;
#14272 = CARTESIAN_POINT ( 'NONE',  ( -6.517576446443361426, -14.80457171870128974, 57.00231026484399166 ) ) ;
#14273 = ORIENTED_EDGE ( 'NONE', *, *, #2694, .T. ) ;
#14274 = VERTEX_POINT ( 'NONE', #14523 ) ;
#14275 = FACE_OUTER_BOUND ( 'NONE', #801, .T. ) ;
#14276 = LINE ( 'NONE', #3793, #8103 ) ;
#14277 = ORIENTED_EDGE ( 'NONE', *, *, #8077, .F. ) ;
#14278 =( LENGTH_UNIT ( ) NAMED_UNIT ( * ) SI_UNIT ( .MILLI., .METRE. ) );
#14279 = VECTOR ( 'NONE', #6064, 1000.000000000000114 ) ;
#14280 = DIRECTION ( 'NONE',  ( 0.5975035461963188466, 0.8018662683283437342, 0.000000000000000000 ) ) ;
#14281 = VECTOR ( 'NONE', #14823, 1000.000000000000000 ) ;
#14282 = EDGE_CURVE ( 'NONE', #1866, #2020, #7692, .T. ) ;
#14283 = DIRECTION ( 'NONE',  ( -1.000000000000000078E-15, 0.05233595624294315463, 0.9986295347545739443 ) ) ;
#14284 = CARTESIAN_POINT ( 'NONE',  ( -15.64858178355719964, -107.1622034095870077, -6.087689735155999315 ) ) ;
#14285 = DIRECTION ( 'NONE',  ( 0.5401126942952622079, 0.8415927028326187775, -6.975647374412502487E-17 ) ) ;
#14286 = ADVANCED_FACE ( 'NONE', ( #13528 ), #6543, .F. ) ;
#14287 = ORIENTED_EDGE ( 'NONE', *, *, #10761, .F. ) ;
#14288 = CARTESIAN_POINT ( 'NONE',  ( 2.500300139188999626, -46.50737899243799944, 16.50231026484399877 ) ) ;
#14289 = DIRECTION ( 'NONE',  ( 0.000000000000000000, 0.000000000000000000, 1.000000000000000000 ) ) ;
#14290 = EDGE_LOOP ( 'NONE', ( #7105, #2169, #1849, #3574 ) ) ;
#14291 = CARTESIAN_POINT ( 'NONE',  ( -15.49969986081099016, -27.00737899243800300, 27.50231026484399877 ) ) ;
#14292 = CARTESIAN_POINT ( 'NONE',  ( -7.754954776104139746, -46.50766419030464505, -2.997807438439666239 ) ) ;
#14293 = ORIENTED_EDGE ( 'NONE', *, *, #9823, .T. ) ;
#14294 = LINE ( 'NONE', #9310, #7415 ) ;
#14295 = ORIENTED_EDGE ( 'NONE', *, *, #3666, .T. ) ;
#14296 = DIRECTION ( 'NONE',  ( -8.018662683283438208E-16, 5.975035461963189015E-16, 1.000000000000000000 ) ) ;
#14297 = VECTOR ( 'NONE', #7788, 1000.000000000000000 ) ;
#14298 = PLANE ( 'NONE',  #15026 ) ;
#14299 = DIRECTION ( 'NONE',  ( -0.9183863840214729901, -0.3956847857120157075, -4.999999999999999402E-16 ) ) ;
#14300 = EDGE_CURVE ( 'NONE', #13801, #5828, #11152, .T. ) ;
#14301 = CARTESIAN_POINT ( 'NONE',  ( -23.55378106252664239, -12.92169478045303066, 57.00231026484397745 ) ) ;
#14302 = EDGE_CURVE ( 'NONE', #14910, #150, #14411, .T. ) ;
#14303 = DIRECTION ( 'NONE',  ( -8.018662683283438208E-16, 5.975035461963189015E-16, 1.000000000000000000 ) ) ;
#14304 = EDGE_CURVE ( 'NONE', #9332, #3162, #14594, .T. ) ;
#14305 = ORIENTED_EDGE ( 'NONE', *, *, #6434, .F. ) ;
#14306 = CARTESIAN_POINT ( 'NONE',  ( -9.152138177982815037, -49.38359113951253221, -17.45695168481910287 ) ) ;
#14307 = DIRECTION ( 'NONE',  ( 1.000000000000000000, 1.201369187114119994E-15, 9.616040805000176517E-16 ) ) ;
#14308 = CARTESIAN_POINT ( 'NONE',  ( -15.49969986081099904, 22.99262100756200411, 8.587064221501004013 ) ) ;
#14309 = ORIENTED_EDGE ( 'NONE', *, *, #7452, .F. ) ;
#14310 = CARTESIAN_POINT ( 'NONE',  ( -18.93133274217424855, -21.90887563098697655, 57.00231026484399166 ) ) ;
#14311 = EDGE_LOOP ( 'NONE', ( #6644, #11386 ) ) ;
#14313 = VERTEX_POINT ( 'NONE', #10999 ) ;
#14312 = DIRECTION ( 'NONE',  ( -8.018662683283439195E-16, 5.975035461963190001E-16, 1.000000000000000000 ) ) ;
#14314 = ADVANCED_FACE ( 'NONE', ( #7546 ), #7621, .T. ) ;
#14315 = ORIENTED_EDGE ( 'NONE', *, *, #2459, .F. ) ;
#14316 = DIRECTION ( 'NONE',  ( 0.05771543059946734194, -0.9983330752162417054, 6.427876096865391919E-16 ) ) ;
#14317 = DIRECTION ( 'NONE',  ( 0.5975035461963188466, 0.8018662683283437342, 0.000000000000000000 ) ) ;
#14318 = LINE ( 'NONE', #9937, #5259 ) ;
#14319 = AXIS2_PLACEMENT_3D ( 'NONE', #12991, #212, #13221 ) ;
#14320 = EDGE_CURVE ( 'NONE', #14012, #7355, #1739, .T. ) ;
#14321 = LINE ( 'NONE', #1236, #2216 ) ;
#14322 = SHAPE_DEFINITION_REPRESENTATION ( #8842, #10770 ) ;
#14323 = ADVANCED_FACE ( 'NONE', ( #600 ), #668, .T. ) ;
#14324 = CARTESIAN_POINT ( 'NONE',  ( -16.95049030215496089, -9.237476495170920288, -13.26085252337267484 ) ) ;
#14325 = DIRECTION ( 'NONE',  ( -0.5975035461963187355, -0.8018662683283439563, 0.000000000000000000 ) ) ;
#14326 = ORIENTED_EDGE ( 'NONE', *, *, #5698, .F. ) ;
#14327 = DIRECTION ( 'NONE',  ( 0.000000000000000000, -1.000000000000000000, -1.224646799147350002E-16 ) ) ;
#14328 = ORIENTED_EDGE ( 'NONE', *, *, #1334, .F. ) ;
#14329 = AXIS2_PLACEMENT_3D ( 'NONE', #12789, #4667, #13999 ) ;
#14330 = FACE_OUTER_BOUND ( 'NONE', #3731, .T. ) ;
#14331 = ORIENTED_EDGE ( 'NONE', *, *, #4, .T. ) ;
#14332 = ORIENTED_EDGE ( 'NONE', *, *, #14916, .F. ) ;
#14333 = CARTESIAN_POINT ( 'NONE',  ( -10.11292913755864475, -19.52351987967747959, 57.00231026484399166 ) ) ;
#14334 = ORIENTED_EDGE ( 'NONE', *, *, #378, .T. ) ;
#14335 = ORIENTED_EDGE ( 'NONE', *, *, #960, .T. ) ;
#14336 = CARTESIAN_POINT ( 'NONE',  ( -15.49969986081092088, -13.50737899243822504, 56.85231026484398598 ) ) ;
#14337 = CYLINDRICAL_SURFACE ( 'NONE', #79, 3.249999999999999556 ) ;
#14338 = PLANE ( 'NONE',  #3188 ) ;
#14339 = FACE_BOUND ( 'NONE', #7560, .T. ) ;
#14340 = CIRCLE ( 'NONE', #7970, 9.974999999999999645 ) ;
#14341 = EDGE_CURVE ( 'NONE', #1981, #10256, #7769, .T. ) ;
#14342 = AXIS2_PLACEMENT_3D ( 'NONE', #8352, #11801, #3065 ) ;
#14343 = DIRECTION ( 'NONE',  ( 0.000000000000000000, 1.000000000000000000, 1.224646799147350002E-16 ) ) ;
#14344 = CARTESIAN_POINT ( 'NONE',  ( -7.869402401354462562, -47.25089185753165566, -3.093175506660042817 ) ) ;
#14345 = ORIENTED_EDGE ( 'NONE', *, *, #5030, .T. ) ;
#14346 = LINE ( 'NONE', #1186, #3126 ) ;
#14347 = DIRECTION ( 'NONE',  ( 0.000000000000000000, 0.000000000000000000, 1.000000000000000000 ) ) ;
#14348 = ORIENTED_EDGE ( 'NONE', *, *, #10669, .T. ) ;
#14349 = ORIENTED_EDGE ( 'NONE', *, *, #13939, .T. ) ;
#14350 = CARTESIAN_POINT ( 'NONE',  ( 22.00028543145668536, -30.25720928778257246, 23.99491965613809086 ) ) ;
#14351 = DIRECTION ( 'NONE',  ( 1.000000000000000000, -1.291538348938060198E-32, 1.054621095516909827E-16 ) ) ;
#14352 = AXIS2_PLACEMENT_3D ( 'NONE', #1297, #463, #7328 ) ;
#14353 = ORIENTED_EDGE ( 'NONE', *, *, #1666, .T. ) ;
#14354 = LINE ( 'NONE', #1780, #14761 ) ;
#14355 = EDGE_CURVE ( 'NONE', #3470, #11437, #4398, .T. ) ;
#14356 = EDGE_CURVE ( 'NONE', #11202, #10535, #11231, .T. ) ;
#14357 =( GEOMETRIC_REPRESENTATION_CONTEXT ( 3 ) GLOBAL_UNCERTAINTY_ASSIGNED_CONTEXT ( ( #8755 ) ) GLOBAL_UNIT_ASSIGNED_CONTEXT ( ( #7393, #13155, #11998 ) ) REPRESENTATION_CONTEXT ( 'NONE', 'WORKASPACE' ) );
#14358 = LINE ( 'NONE', #12988, #3411 ) ;
#14359 = CARTESIAN_POINT ( 'NONE',  ( -10.98945933209236969, -22.43249828447867245, 56.73009184860239884 ) ) ;
#14360 = VECTOR ( 'NONE', #8704, 1000.000000000000000 ) ;
#14361 = CARTESIAN_POINT ( 'NONE',  ( -7.512172356294475328, -44.98005919120003426, 17.52071913701680828 ) ) ;
#14362 = DIRECTION ( 'NONE',  ( 3.632077277826439854E-16, -1.000000000000000000, 0.000000000000000000 ) ) ;
#14363 = AXIS2_PLACEMENT_3D ( 'NONE', #10813, #2846, #13486 ) ;
#14364 = ORIENTED_EDGE ( 'NONE', *, *, #5321, .T. ) ;
#14365 = DIRECTION ( 'NONE',  ( 0.5975035461963189576, 0.8018662683283437342, 0.000000000000000000 ) ) ;
#14366 = DIRECTION ( 'NONE',  ( 0.5975035461963189576, 0.8018662683283437342, 0.000000000000000000 ) ) ;
#14367 = ORIENTED_EDGE ( 'NONE', *, *, #3691, .T. ) ;
#14368 = LINE ( 'NONE', #2586, #14887 ) ;
#14369 = FILL_AREA_STYLE_COLOUR ( '', #7734 ) ;
#14370 = VERTEX_POINT ( 'NONE', #12607 ) ;
#14371 = DIRECTION ( 'NONE',  ( 0.6251242923673534513, 0.7805252200231685977, 3.489949670250099574E-17 ) ) ;
#14372 = CARTESIAN_POINT ( 'NONE',  ( -7.754930580632606762, -46.50765881518451295, 22.00225574842814424 ) ) ;
#14373 = ADVANCED_FACE ( 'NONE', ( #8069 ), #3272, .F. ) ;
#14374 = VECTOR ( 'NONE', #5051, 1000.000000000000000 ) ;
#14375 = VECTOR ( 'NONE', #6139, 1000.000000000000114 ) ;
#14376 = VECTOR ( 'NONE', #8793, 1000.000000000000000 ) ;
#14377 = LINE ( 'NONE', #3891, #12038 ) ;
#14378 = CARTESIAN_POINT ( 'NONE',  ( -7.773685182324180154, -47.89679818372218278, 17.41897699471824623 ) ) ;
#14379 = CARTESIAN_POINT ( 'NONE',  ( 18.44182102609496354, -28.13808047628806719, 8.267357603750861372 ) ) ;
#14380 = CARTESIAN_POINT ( 'NONE',  ( -6.540243082598547808, -14.95284924095401458, 57.00231026484399166 ) ) ;
#14381 = VERTEX_POINT ( 'NONE', #12840 ) ;
#14382 = CARTESIAN_POINT ( 'NONE',  ( -7.551915124174499283, -45.55891546459999830, -17.14593156766008164 ) ) ;
#14383 = LINE ( 'NONE', #12236, #10199 ) ;
#14384 = ORIENTED_EDGE ( 'NONE', *, *, #7187, .F. ) ;
#14385 = LINE ( 'NONE', #14310, #3466 ) ;
#14386 = ORIENTED_EDGE ( 'NONE', *, *, #8312, .F. ) ;
#14388 = VERTEX_POINT ( 'NONE', #5552 ) ;
#14387 = CARTESIAN_POINT ( 'NONE',  ( -8.744338604334316756, -15.61126689213601360, 56.85231026484400019 ) ) ;
#14389 = ORIENTED_EDGE ( 'NONE', *, *, #333, .T. ) ;
#14390 = EDGE_CURVE ( 'NONE', #1143, #4490, #10224, .T. ) ;
#14391 = CARTESIAN_POINT ( 'NONE',  ( -20.87112600995945755, -108.0608273576312968, -5.497689735156002122 ) ) ;
#14392 = DIRECTION ( 'NONE',  ( 1.445602896647339656E-16, 0.000000000000000000, -1.000000000000000000 ) ) ;
#14393 = EDGE_CURVE ( 'NONE', #13485, #11236, #14897, .T. ) ;
#14394 = DIRECTION ( 'NONE',  ( -0.6601155939154559338, 0.7511640317997426708, -9.781476007338054812E-16 ) ) ;
#14395 = CARTESIAN_POINT ( 'NONE',  ( -12.27197285165629737, -4.041276922754793333, 61.57424106746455550 ) ) ;
#14396 = APPLICATION_PROTOCOL_DEFINITION ( 'draft international standard', 'automotive_design', 1998, #14753 ) ;
#14397 = PLANE ( 'NONE',  #13640 ) ;
#14398 = VECTOR ( 'NONE', #12851, 1000.000000000000227 ) ;
#14399 = LINE ( 'NONE', #11681, #8721 ) ;
#14400 = DIRECTION ( 'NONE',  ( -8.018662683283438208E-16, 5.975035461963189015E-16, 1.000000000000000000 ) ) ;
#14401 = CARTESIAN_POINT ( 'NONE',  ( -15.49969986081099904, 4.873818854045002702, 1.212064221501000461 ) ) ;
#14402 = ORIENTED_EDGE ( 'NONE', *, *, #8789, .T. ) ;
#14403 = CARTESIAN_POINT ( 'NONE',  ( -7.307539508764906877, -16.04208977798462854, 57.00231026484399166 ) ) ;
#14404 = ORIENTED_EDGE ( 'NONE', *, *, #7834, .T. ) ;
#14405 = ORIENTED_EDGE ( 'NONE', *, *, #4454, .T. ) ;
#14406 = EDGE_CURVE ( 'NONE', #1735, #10639, #13677, .T. ) ;
#14407 = FACE_OUTER_BOUND ( 'NONE', #12054, .T. ) ;
#14408 = EDGE_CURVE ( 'NONE', #11422, #8216, #7921, .T. ) ;
#14409 = VERTEX_POINT ( 'NONE', #6766 ) ;
#14410 = DIRECTION ( 'NONE',  ( -0.1165201156931293391, -0.9931883319083343320, 4.999999999999998416E-16 ) ) ;
#14411 = CIRCLE ( 'NONE', #9764, 9.974999999999999645 ) ;
#14412 = DIRECTION ( 'NONE',  ( 0.000000000000000000, 0.000000000000000000, 1.000000000000000000 ) ) ;
#14413 = DIRECTION ( 'NONE',  ( 0.9472588896649083434, -0.3204693369899919708, 9.510565162951537596E-16 ) ) ;
#14414 = DIRECTION ( 'NONE',  ( -3.660254037844389484E-16, 0.8386705679454246054, -0.5446390350150263071 ) ) ;
#14416 = CARTESIAN_POINT ( 'NONE',  ( -38.20013690429809827, 4.873818854045000037, 20.51204286552489009 ) ) ;
#14415 = DIRECTION ( 'NONE',  ( 0.9988970074402869770, -0.04695496274984588270, 8.290375725550417844E-16 ) ) ;
#14417 = ORIENTED_EDGE ( 'NONE', *, *, #7017, .F. ) ;
#14418 = DIRECTION ( 'NONE',  ( -0.000000000000000000, 1.000000000000000000, 0.000000000000000000 ) ) ;
#14419 = ORIENTED_EDGE ( 'NONE', *, *, #354, .T. ) ;
#14420 = DIRECTION ( 'NONE',  ( -0.9183863840214729901, -0.3956847857120157075, -4.999999999999999402E-16 ) ) ;
#14421 = VERTEX_POINT ( 'NONE', #11451 ) ;
#14422 = ORIENTED_EDGE ( 'NONE', *, *, #9633, .T. ) ;
#14423 = CARTESIAN_POINT ( 'NONE',  ( 21.86100802344563832, -27.43036982981187677, 20.98262938449914117 ) ) ;
#14424 = DIRECTION ( 'NONE',  ( -0.6251242923673536733, -0.7805252200231682647, -3.489949670250128540E-17 ) ) ;
#14425 = ADVANCED_FACE ( 'NONE', ( #12761 ), #6989, .F. ) ;
#14426 = ORIENTED_EDGE ( 'NONE', *, *, #2403, .T. ) ;
#14427 = LINE ( 'NONE', #13295, #2199 ) ;
#14428 = DIRECTION ( 'NONE',  ( 8.018662683283438208E-16, -5.975035461963189015E-16, -1.000000000000000000 ) ) ;
#14429 = EDGE_CURVE ( 'NONE', #2863, #11333, #5630, .T. ) ;
#14430 = DIRECTION ( 'NONE',  ( -0.7032868978765995926, -0.7109061395677416240, -1.391731009600651544E-16 ) ) ;
#14431 = DIRECTION ( 'NONE',  ( -8.018662683283438208E-16, 5.975035461963189015E-16, 1.000000000000000000 ) ) ;
#14432 = ORIENTED_EDGE ( 'NONE', *, *, #12487, .F. ) ;
#14433 = DIRECTION ( 'NONE',  ( 0.9183863840214729901, 0.3956847857120157075, 5.000000000000000389E-16 ) ) ;
#14434 = PLANE ( 'NONE',  #12889 ) ;
#14435 = ORIENTED_EDGE ( 'NONE', *, *, #3341, .F. ) ;
#14436 = B_SPLINE_CURVE_WITH_KNOTS ( 'NONE', 3,
 ( #7493, #11017, #7421, #2836 ),
 .UNSPECIFIED., .F., .F.,
 ( 4, 4 ),
 ( 0.000000000000000000, 0.1213360741398818166 ),
 .UNSPECIFIED. ) ;
#14437 = CARTESIAN_POINT ( 'NONE',  ( 21.86816044869649289, -26.16306096081211052, 21.06647100910851123 ) ) ;
#14438 = DIRECTION ( 'NONE',  ( 0.000000000000000000, -1.000000000000000000, -1.224646799147350002E-16 ) ) ;
#14439 = ORIENTED_EDGE ( 'NONE', *, *, #8012, .F. ) ;
#14440 = CARTESIAN_POINT ( 'NONE',  ( -28.78282149594069850, -31.14135358865360104, 59.28069236156870403 ) ) ;
#14441 = ORIENTED_EDGE ( 'NONE', *, *, #12915, .T. ) ;
#14442 = CARTESIAN_POINT ( 'NONE',  ( -11.71495923925436955, -5.812446346369147143, 57.00231026484397745 ) ) ;
#14443 = CIRCLE ( 'NONE', #14930, 9.974999999999999645 ) ;
#14444 = LINE ( 'NONE', #4897, #5189 ) ;
#14445 = DIRECTION ( 'NONE',  ( 0.000000000000000000, 0.000000000000000000, -1.000000000000000000 ) ) ;
#14446 = EDGE_CURVE ( 'NONE', #8466, #8073, #976, .T. ) ;
#14447 = CARTESIAN_POINT ( 'NONE',  ( 17.02627693417459298, -30.24626016961038744, 5.547585651947908758 ) ) ;
#14448 = DIRECTION ( 'NONE',  ( 1.000000000000000000, 0.000000000000000000, 0.000000000000000000 ) ) ;
#14449 = ORIENTED_EDGE ( 'NONE', *, *, #6252, .F. ) ;
#14450 = CARTESIAN_POINT ( 'NONE',  ( -12.92091935695870042, -52.08489029401035708, -17.90976127491029146 ) ) ;
#14451 = EDGE_CURVE ( 'NONE', #14119, #7812, #14970, .T. ) ;
#14452 = CARTESIAN_POINT ( 'NONE',  ( -34.37762275815202173, -39.17044586891318403, 51.90428018001587418 ) ) ;
#14453 = VECTOR ( 'NONE', #791, 1000.000000000000227 ) ;
#14454 = ORIENTED_EDGE ( 'NONE', *, *, #4988, .T. ) ;
#14455 = VERTEX_POINT ( 'NONE', #4495 ) ;
#14457 = ORIENTED_EDGE ( 'NONE', *, *, #12824, .F. ) ;
#14456 = CARTESIAN_POINT ( 'NONE',  ( -35.14379750997561302, -38.30087877078398151, -12.44075990407947607 ) ) ;
#14458 = ORIENTED_EDGE ( 'NONE', *, *, #4190, .T. ) ;
#14459 = DIRECTION ( 'NONE',  ( -0.9354976265738682573, 0.3533329742249642913, -9.612616959383187437E-16 ) ) ;
#14460 = LINE ( 'NONE', #401, #2667 ) ;
#14461 = VECTOR ( 'NONE', #2404, 1000.000000000000000 ) ;
#14462 = CARTESIAN_POINT ( 'NONE',  ( -15.49969986081093509, -96.50737899243799234, -0.1262635860074601546 ) ) ;
#14463 = VECTOR ( 'NONE', #7501, 1000.000000000000000 ) ;
#14464 = CARTESIAN_POINT ( 'NONE',  ( -15.49969986081092088, -13.50737899243822504, 57.00231026484397745 ) ) ;
#14465 = CARTESIAN_POINT ( 'NONE',  ( 13.85920135429429934, -27.00737899243800300, 7.712064221501001349 ) ) ;
#14466 = EDGE_CURVE ( 'NONE', #775, #13889, #7792, .T. ) ;
#14467 = CARTESIAN_POINT ( 'NONE',  ( -33.49969986081099904, -37.00737899243799944, 19.50231026484398811 ) ) ;
#14468 = EDGE_CURVE ( 'NONE', #6205, #11933, #13973, .T. ) ;
#14469 = CIRCLE ( 'NONE', #13261, 9.974999999999999645 ) ;
#14470 = ORIENTED_EDGE ( 'NONE', *, *, #9314, .T. ) ;
#14471 = DIRECTION ( 'NONE',  ( -1.054621095516909827E-16, 1.224646799147350002E-16, -1.000000000000000000 ) ) ;
#14472 = CIRCLE ( 'NONE', #3475, 1.249999999999999778 ) ;
#14473 = ORIENTED_EDGE ( 'NONE', *, *, #3928, .T. ) ;
#14474 = DIRECTION ( 'NONE',  ( 1.000000000000000000, 0.000000000000000000, 1.011922027653137537E-15 ) ) ;
#14475 = VERTEX_POINT ( 'NONE', #2276 ) ;
#14476 = EDGE_LOOP ( 'NONE', ( #13017, #12951 ) ) ;
#14477 = AXIS2_PLACEMENT_3D ( 'NONE', #10292, #10216, #3187 ) ;
#14478 = VECTOR ( 'NONE', #5614, 999.9999999999998863 ) ;
#14479 = CARTESIAN_POINT ( 'NONE',  ( -1.508527451665002017, -44.04887899243799154, -5.497689735156000346 ) ) ;
#14480 = EDGE_LOOP ( 'NONE', ( #13482, #1169, #12136, #2585 ) ) ;
#14481 = CARTESIAN_POINT ( 'NONE',  ( -7.734307812155742923, -7.246443652516327383, 56.85231026484400019 ) ) ;
#14482 = CARTESIAN_POINT ( 'NONE',  ( -20.06719866676104402, -21.34952185377683165, 56.85231026484398598 ) ) ;
#14483 = DIRECTION ( 'NONE',  ( 0.2640193276337003403, -0.9645173894937555392, 7.880107536067285830E-16 ) ) ;
#14484 = VECTOR ( 'NONE', #12740, 1000.000000000000000 ) ;
#14485 = VECTOR ( 'NONE', #2014, 1000.000000000000114 ) ;
#14486 = EDGE_CURVE ( 'NONE', #14455, #9903, #6567, .T. ) ;
#14487 = EDGE_CURVE ( 'NONE', #10256, #2967, #13202, .T. ) ;
#14489 = CARTESIAN_POINT ( 'NONE',  ( -23.68291657637574588, -19.21137664199072148, 56.85231026484398598 ) ) ;
#14488 = CARTESIAN_POINT ( 'NONE',  ( -15.49969986081099727, -27.00737899243800300, 2.502310264843997878 ) ) ;
#14490 = EDGE_CURVE ( 'NONE', #6732, #4531, #15042, .T. ) ;
#14491 = VERTEX_POINT ( 'NONE', #1120 ) ;
#14492 = CARTESIAN_POINT ( 'NONE',  ( -15.49969986081099904, -57.00737899243800655, 19.50231026484399877 ) ) ;
#14493 = CARTESIAN_POINT ( 'NONE',  ( -15.49969986081099904, 37.56536188261469533, 18.96206422150100224 ) ) ;
#14494 = EDGE_LOOP ( 'NONE', ( #1017, #13914, #2435, #5896 ) ) ;
#14495 = VERTEX_POINT ( 'NONE', #10453 ) ;
#14496 = LINE ( 'NONE', #3943, #10064 ) ;
#14497 = CARTESIAN_POINT ( 'NONE',  ( -20.79164517123715683, -50.52944030466328940, 56.62889509689365042 ) ) ;
#14498 = ORIENTED_EDGE ( 'NONE', *, *, #1134, .T. ) ;
#14499 = EDGE_CURVE ( 'NONE', #2398, #11181, #15116, .T. ) ;
#14500 = AXIS2_PLACEMENT_3D ( 'NONE', #1567, #5092, #4790 ) ;
#14501 = CARTESIAN_POINT ( 'NONE',  ( 0.8003001391889992266, 11.99262100756199878, 32.26206422150099939 ) ) ;
#14502 = CIRCLE ( 'NONE', #12297, 9.974999999999999645 ) ;
#14503 = VECTOR ( 'NONE', #6308, 1000.000000000000000 ) ;
#14504 = VECTOR ( 'NONE', #9209, 1000.000000000000000 ) ;
#14505 = CARTESIAN_POINT ( 'NONE',  ( -20.60655739512266749, -107.1622034095862972, -7.162689735156005710 ) ) ;
#14506 = ADVANCED_FACE ( 'NONE', ( #1428 ), #1692, .F. ) ;
#14507 = B_SPLINE_CURVE_WITH_KNOTS ( 'NONE', 3,
 ( #7173, #6179, #12008, #8632, #14379, #7476, #460, #14152, #7326, #12151, #3895, #4902, #5047, #3745, #1450, #14447, #8554, #13015, #10861, #7404, #6326, #1527, #5190, #10782, #13165, #2597, #9783, #13316, #3972, #8323, #11852, #12085, #13239, #3672 ),
 .UNSPECIFIED., .F., .F.,
 ( 4, 2, 2, 2, 2, 2, 2, 2, 2, 2, 2, 2, 2, 2, 2, 2, 4 ),
 ( 0.000000000000000000, 0.0006891453135227206461, 0.001378290627045441292, 0.002067435940568161830, 0.002756581254090882584, 0.003445726567613603773, 0.004134871881136323660, 0.004824017194659043981, 0.005513162508181765169, 0.006202307821704486357, 0.006891453135227207545, 0.007580598448749926131, 0.008269743762272647319, 0.008958889075795369375, 0.009648034389318091431, 0.01033717970284081349, 0.01102632501636353554 ),
 .UNSPECIFIED. ) ;
#14508 = DIRECTION ( 'NONE',  ( 0.000000000000000000, 1.000000000000000000, 1.224646799147350002E-16 ) ) ;
#14509 = ADVANCED_FACE ( 'NONE', ( #8533 ), #4878, .T. ) ;
#14510 = VECTOR ( 'NONE', #8766, 1000.000000000000114 ) ;
#14511 = FACE_OUTER_BOUND ( 'NONE', #2610, .T. ) ;
#14512 = ORIENTED_EDGE ( 'NONE', *, *, #12043, .T. ) ;
#14513 = LINE ( 'NONE', #10054, #3851 ) ;
#14514 = DIRECTION ( 'NONE',  ( 8.018662683283438208E-16, -5.975035461963189015E-16, -1.000000000000000000 ) ) ;
#14515 = ORIENTED_EDGE ( 'NONE', *, *, #4397, .T. ) ;
#14516 = CARTESIAN_POINT ( 'NONE',  ( 21.87338300223960985, -25.95928379819316234, 27.29579227643073835 ) ) ;
#14517 =( NAMED_UNIT ( * ) PLANE_ANGLE_UNIT ( ) SI_UNIT ( $, .RADIAN. ) );
#14518 = ORIENTED_EDGE ( 'NONE', *, *, #4624, .F. ) ;
#14519 = LINE ( 'NONE', #9851, #11077 ) ;
#14520 = CIRCLE ( 'NONE', #9631, 9.974999999999999645 ) ;
#14521 = ORIENTED_EDGE ( 'NONE', *, *, #11827, .T. ) ;
#14522 = EDGE_CURVE ( 'NONE', #7227, #7782, #3722, .T. ) ;
#14523 = CARTESIAN_POINT ( 'NONE',  ( -13.16883223745437448, -21.23902216335526916, 56.85231026484400019 ) ) ;
#14524 = CARTESIAN_POINT ( 'NONE',  ( -7.707857435417036385, -48.23250629231411324, 17.69147438052686994 ) ) ;
#14525 = VECTOR ( 'NONE', #1254, 1000.000000000000000 ) ;
#14526 = DIRECTION ( 'NONE',  ( -8.018662683283438208E-16, 5.975035461963189015E-16, 1.000000000000000000 ) ) ;
#14527 = DIRECTION ( 'NONE',  ( 0.000000000000000000, 1.000000000000000000, 1.224646799147350002E-16 ) ) ;
#14528 = ORIENTED_EDGE ( 'NONE', *, *, #5445, .T. ) ;
#14529 = DIRECTION ( 'NONE',  ( 8.018662683283438208E-16, -5.975035461963189015E-16, -1.000000000000000000 ) ) ;
#14530 = CARTESIAN_POINT ( 'NONE',  ( -9.328067836852527606, -18.71527762440592468, 57.00231026484399166 ) ) ;
#14531 = VECTOR ( 'NONE', #1722, 1000.000000000000114 ) ;
#14532 = VERTEX_POINT ( 'NONE', #7147 ) ;
#14533 = VERTEX_POINT ( 'NONE', #8376 ) ;
#14535 = EDGE_LOOP ( 'NONE', ( #5481, #13856, #2501, #5585 ) ) ;
#14534 = CARTESIAN_POINT ( 'NONE',  ( -34.94125367352354061, -38.49305635555177929, -12.56456997079345506 ) ) ;
#14536 = ORIENTED_EDGE ( 'NONE', *, *, #9534, .F. ) ;
#14537 = LINE ( 'NONE', #2686, #14244 ) ;
#14538 = DIRECTION ( 'NONE',  ( 1.000000000000000000, -1.291538348938060198E-32, 1.054621095516909827E-16 ) ) ;
#14539 = EDGE_CURVE ( 'NONE', #2347, #11156, #3653, .T. ) ;
#14540 = ADVANCED_FACE ( 'NONE', ( #8227 ), #7380, .T. ) ;
#14541 = LINE ( 'NONE', #4058, #6639 ) ;
#14542 = CARTESIAN_POINT ( 'NONE',  ( -33.23672817421918779, 7.708027139131385930, 17.39831465307906555 ) ) ;
#14543 = AXIS2_PLACEMENT_3D ( 'NONE', #785, #14706, #8957 ) ;
#14544 = LINE ( 'NONE', #5355, #6108 ) ;
#14545 = CARTESIAN_POINT ( 'NONE',  ( -7.512805849530849400, -44.04964101872670312, 19.04457229113268113 ) ) ;
#14546 = FACE_OUTER_BOUND ( 'NONE', #5793, .T. ) ;
#14547 = PLANE ( 'NONE',  #4723 ) ;
#14548 = EDGE_LOOP ( 'NONE', ( #3747, #11720, #5938, #13578 ) ) ;
#14549 = CARTESIAN_POINT ( 'NONE',  ( -7.499699860810999041, -19.50737899243799589, 6.712064221500998684 ) ) ;
#14550 = ORIENTED_EDGE ( 'NONE', *, *, #7938, .F. ) ;
#14551 = CARTESIAN_POINT ( 'NONE',  ( -20.00744539586189319, -5.630737564061013778, 57.00231026484397745 ) ) ;
#14553 = ORIENTED_EDGE ( 'NONE', *, *, #393, .T. ) ;
#14552 = CARTESIAN_POINT ( 'NONE',  ( -7.517675258046085496, -45.05616182903360567, -7.535809151347679702 ) ) ;
#14554 = VERTEX_POINT ( 'NONE', #5101 ) ;
#14555 = CARTESIAN_POINT ( 'NONE',  ( -14.26755283655060680, -21.48817241857114269, 57.00231026484399166 ) ) ;
#14556 = ORIENTED_EDGE ( 'NONE', *, *, #5314, .F. ) ;
#14557 = DIRECTION ( 'NONE',  ( -1.000000000000000000, -1.201369187114119994E-15, -9.616040805000176517E-16 ) ) ;
#14558 = ADVANCED_FACE ( 'NONE', ( #3569 ), #9608, .F. ) ;
#14559 = CARTESIAN_POINT ( 'NONE',  ( -15.49969986081092088, -13.50737899243822504, 57.00231026484397745 ) ) ;
#14560 = CARTESIAN_POINT ( 'NONE',  ( -15.49969986081099371, -2.007378992437995890, -13.28793577849899243 ) ) ;
#14561 = VECTOR ( 'NONE', #9859, 1000.000000000000000 ) ;
#14563 = CARTESIAN_POINT ( 'NONE',  ( -34.68296123826191035, 6.562241739503763327, 18.28527686625572457 ) ) ;
#14562 = CARTESIAN_POINT ( 'NONE',  ( -14.19354049678269192, -21.47604090745013750, 56.85231026484400019 ) ) ;
#14564 = VERTEX_POINT ( 'NONE', #2576 ) ;
#14565 = CARTESIAN_POINT ( 'NONE',  ( -38.49969986081099904, -42.00737899243800655, 19.50231026484398811 ) ) ;
#14566 = EDGE_LOOP ( 'NONE', ( #2100, #8763, #3442, #11031, #13756, #10827, #12407, #5258, #10962 ) ) ;
#14567 = CARTESIAN_POINT ( 'NONE',  ( -2.216578225681298697, -32.00737899243799944, -11.04189727591769632 ) ) ;
#14568 = ORIENTED_EDGE ( 'NONE', *, *, #97, .T. ) ;
#14569 = ORIENTED_EDGE ( 'NONE', *, *, #10780, .F. ) ;
#14570 = CARTESIAN_POINT ( 'NONE',  ( 21.87337189122190040, -28.05484980333040923, 21.12821865650454711 ) ) ;
#14571 = CARTESIAN_POINT ( 'NONE',  ( 0.8003001391889992266, 20.99262100756200056, 32.26206422150099939 ) ) ;
#14572 = ORIENTED_EDGE ( 'NONE', *, *, #7898, .T. ) ;
#14573 = PLANE ( 'NONE',  #13981 ) ;
#14574 = EDGE_CURVE ( 'NONE', #5848, #10870, #10739, .T. ) ;
#14575 = EDGE_CURVE ( 'NONE', #11915, #11355, #2427, .T. ) ;
#14576 = CARTESIAN_POINT ( 'NONE',  ( -14.61203582817000246, -106.1798807882712765, -5.562105325730671623 ) ) ;
#14577 = CARTESIAN_POINT ( 'NONE',  ( 6.045543233663400073, 12.99262100756199878, 32.26206422150099939 ) ) ;
#14578 = CARTESIAN_POINT ( 'NONE',  ( -10.70529993155776083, -22.28872569541405113, 56.69565590118975962 ) ) ;
#14579 = EDGE_CURVE ( 'NONE', #2810, #12214, #7223, .T. ) ;
#14580 = CARTESIAN_POINT ( 'NONE',  ( -25.29546517631142777, -15.38982603914036318, 54.00231026484397745 ) ) ;
#14581 = CARTESIAN_POINT ( 'NONE',  ( -10.96544185377836911, -6.825182173602284408, 56.85231026484398598 ) ) ;
#14582 = ORIENTED_EDGE ( 'NONE', *, *, #3646, .T. ) ;
#14583 = FACE_OUTER_BOUND ( 'NONE', #5455, .T. ) ;
#14584 = CIRCLE ( 'NONE', #4321, 37.50000000000000711 ) ;
#14585 = DIRECTION ( 'NONE',  ( -1.000000000000000000, 0.000000000000000000, 0.000000000000000000 ) ) ;
#14586 = EDGE_LOOP ( 'NONE', ( #13873, #2226, #11842, #10992 ) ) ;
#14587 = CARTESIAN_POINT ( 'NONE',  ( 21.87335010765016108, -25.96044300975462349, 21.12793889599969077 ) ) ;
#14588 = LINE ( 'NONE', #14666, #14510 ) ;
#14589 = EDGE_LOOP ( 'NONE', ( #3412, #5213, #8136, #14439 ) ) ;
#14590 = AXIS2_PLACEMENT_3D ( 'NONE', #8044, #32, #9354 ) ;
#14591 = CARTESIAN_POINT ( 'NONE',  ( -7.795056982475612628, -46.66304653480354858, 22.00230981020063581 ) ) ;
#14592 = EDGE_CURVE ( 'NONE', #10777, #3470, #11829, .T. ) ;
#14593 = EDGE_CURVE ( 'NONE', #5527, #1243, #2917, .T. ) ;
#14594 = LINE ( 'NONE', #11229, #493 ) ;
#14595 = VECTOR ( 'NONE', #9862, 1000.000000000000000 ) ;
#14596 = CARTESIAN_POINT ( 'NONE',  ( -10.39628701978575975, -6.002951807498697612, 56.85231026484398598 ) ) ;
#14597 = VECTOR ( 'NONE', #2871, 1000.000000000000000 ) ;
#14598 = DIRECTION ( 'NONE',  ( 8.018662683283438208E-16, -5.975035461963189015E-16, -1.000000000000000000 ) ) ;
#14599 = DIRECTION ( 'NONE',  ( -0.9085715390340232123, 0.4177292884839972631, -9.781476007338056784E-16 ) ) ;
#14600 = ORIENTED_EDGE ( 'NONE', *, *, #10337, .F. ) ;
#14601 = CARTESIAN_POINT ( 'NONE',  ( -32.81697519099675020, 10.05207975130290521, 32.03010237117641168 ) ) ;
#14602 = CARTESIAN_POINT ( 'NONE',  ( -15.49969986081092088, -13.50737899243822504, 56.85231026484398598 ) ) ;
#14603 = ORIENTED_EDGE ( 'NONE', *, *, #1101, .F. ) ;
#14604 = VECTOR ( 'NONE', #9825, 1000.000000000000227 ) ;
#14606 = ORIENTED_EDGE ( 'NONE', *, *, #5926, .T. ) ;
#14605 = CARTESIAN_POINT ( 'NONE',  ( -33.65607387164132547, -40.75537920815241932, -13.30924300046305397 ) ) ;
#14607 = B_SPLINE_CURVE_WITH_KNOTS ( 'NONE', 3,
 ( #6670, #10195, #11577, #3089, #802, #9047, #2099, #6741, #954, #5607, #3620, #187, #9433, #8125, #10734, #10507, #11725, #11962, #2328, #12817, #4699, #6963, #8278, #10581, #116, #14102, #9585, #261, #5902, #2474, #8357, #12887, #11651, #1480, #12969 ),
 .UNSPECIFIED., .F., .F.,
 ( 4, 2, 2, 2, 2, 2, 2, 2, 2, 1, 1, 2, 2, 2, 1, 1, 1, 2, 2, 4 ),
 ( 0.000000000000000000, 0.06250000000000119349, 0.09375000000000185962, 0.1250000000000025258, 0.1875000000000059119, 0.2187500000000087153, 0.2500000000000114908, 0.3750000000000204836, 0.4375000000000254796, 0.4687500000000274780, 0.4843750000000288103, 0.4921875000000295319, 0.5000000000000303091, 0.6250000000000239808, 0.6875000000000202061, 0.7187500000000189848, 0.7343750000000175415, 0.7421875000000172085, 0.7500000000000167644, 1.000000000000000000 ),
 .UNSPECIFIED. ) ;
#14608 = ORIENTED_EDGE ( 'NONE', *, *, #6440, .T. ) ;
#14609 = FACE_OUTER_BOUND ( 'NONE', #14480, .T. ) ;
#14610 = ORIENTED_EDGE ( 'NONE', *, *, #2051, .T. ) ;
#14611 = EDGE_CURVE ( 'NONE', #2532, #8256, #1215, .T. ) ;
#14612 = CYLINDRICAL_SURFACE ( 'NONE', #12776, 37.49999999999999289 ) ;
#14613 = CARTESIAN_POINT ( 'NONE',  ( -6.766506000727597225, -11.03906478995046214, 56.85231026484400019 ) ) ;
#14614 = CARTESIAN_POINT ( 'NONE',  ( -15.49969986081099904, 70.81438635534659909, 24.21206422150100579 ) ) ;
#14615 = VECTOR ( 'NONE', #10552, 1000.000000000000000 ) ;
#14616 = CARTESIAN_POINT ( 'NONE',  ( -23.49646891012291050, -9.216349422280851300, 56.85231026484398598 ) ) ;
#14617 = DIRECTION ( 'NONE',  ( 0.000000000000000000, 9.130123557772668334E-17, -1.000000000000000000 ) ) ;
#14618 = ADVANCED_FACE ( 'NONE', ( #11986 ), #1352, .F. ) ;
#14619 = CARTESIAN_POINT ( 'NONE',  ( -7.506371897368028456, -44.17798263326779562, 43.58480693617389079 ) ) ;
#14620 = ORIENTED_EDGE ( 'NONE', *, *, #12574, .T. ) ;
#14621 = DIRECTION ( 'NONE',  ( 0.5975035461963189576, 0.8018662683283437342, 0.000000000000000000 ) ) ;
#14622 = ORIENTED_EDGE ( 'NONE', *, *, #3311, .F. ) ;
#14623 = CARTESIAN_POINT ( 'NONE',  ( -15.61203582816999713, -107.9151965264422586, -6.615812085103268458 ) ) ;
#14625 = EDGE_LOOP ( 'NONE', ( #9460, #2451, #3717, #165 ) ) ;
#14624 = CARTESIAN_POINT ( 'NONE',  ( -7.593870215980957461, -45.75074864731840307, -7.912782458232928917 ) ) ;
#14626 = ORIENTED_EDGE ( 'NONE', *, *, #12893, .T. ) ;
#14627 =( GEOMETRIC_REPRESENTATION_CONTEXT ( 3 ) GLOBAL_UNCERTAINTY_ASSIGNED_CONTEXT ( ( #11702 ) ) GLOBAL_UNIT_ASSIGNED_CONTEXT ( ( #10339, #9113, #9184 ) ) REPRESENTATION_CONTEXT ( 'NONE', 'WORKASPACE' ) );
#14628 = CARTESIAN_POINT ( 'NONE',  ( -19.38713143869018296, -6.429305403720261936, 57.00231026484397745 ) ) ;
#14630 = ORIENTED_EDGE ( 'NONE', *, *, #5882, .F. ) ;
#14629 = CARTESIAN_POINT ( 'NONE',  ( -10.85342163307452523, -20.71489927548028476, 56.85231026484400019 ) ) ;
#14631 = LINE ( 'NONE', #10891, #14160 ) ;
#14632 = DIRECTION ( 'NONE',  ( 8.018662683283438208E-16, -5.975035461963189015E-16, -1.000000000000000000 ) ) ;
#14633 = CARTESIAN_POINT ( 'NONE',  ( -13.85656510877104353, -11.30224675453528072, 56.75231026484397745 ) ) ;
#14634 = AXIS2_PLACEMENT_3D ( 'NONE', #13988, #1128, #2132 ) ;
#14635 = B_SPLINE_CURVE_WITH_KNOTS ( 'NONE', 3,
 ( #9295, #2117, #8145, #6760, #4794, #7062, #7218, #5921, #13061, #12835, #7142, #9603, #5846, #2570, #1263, #363, #8295, #10755, #2646, #9378, #8220, #4944, #4872 ),
 .UNSPECIFIED., .F., .F.,
 ( 4, 2, 1, 2, 2, 2, 2, 2, 2, 2, 2, 4 ),
 ( 0.01260726791730938309, 0.01339567446202048762, 0.01418408100673159040, 0.01497248755144269493, 0.01576089409615379772, 0.01733770718557600329, 0.01891452027499820887, 0.02049133336442041098, 0.02127973990913151550, 0.02206814645384262003, 0.02364495954326482213, 0.02522177263268702771 ),
 .UNSPECIFIED. ) ;
#14636 = EDGE_CURVE ( 'NONE', #12333, #4377, #14114, .T. ) ;
#14638 = CARTESIAN_POINT ( 'NONE',  ( -35.52696516869671228, 6.159096188266306449, 18.68424166250937901 ) ) ;
#14637 = DIRECTION ( 'NONE',  ( -8.018662683283438208E-16, 5.975035461963189015E-16, 1.000000000000000000 ) ) ;
#14639 = ORIENTED_EDGE ( 'NONE', *, *, #11394, .F. ) ;
#14640 = PLANE ( 'NONE',  #2641 ) ;
#14641 = ORIENTED_EDGE ( 'NONE', *, *, #11730, .T. ) ;
#14642 = EDGE_CURVE ( 'NONE', #11647, #10391, #14358, .T. ) ;
#14643 = CARTESIAN_POINT ( 'NONE',  ( 13.85920135429429934, -27.00737899243800300, 5.212064221501000461 ) ) ;
#14644 = ORIENTED_EDGE ( 'NONE', *, *, #13882, .F. ) ;
#14645 = ORIENTED_EDGE ( 'NONE', *, *, #11931, .T. ) ;
#14646 = CARTESIAN_POINT ( 'NONE',  ( -7.497874475122997318, -44.50608669435617770, -6.993290823733421036 ) ) ;
#14647 = VERTEX_POINT ( 'NONE', #4094 ) ;
#14648 = CIRCLE ( 'NONE', #9995, 2.500000000000002220 ) ;
#14649 = VECTOR ( 'NONE', #6694, 1000.000000000000227 ) ;
#14650 = DIRECTION ( 'NONE',  ( -8.018662683283438208E-16, 5.975035461963189015E-16, 1.000000000000000000 ) ) ;
#14651 = CARTESIAN_POINT ( 'NONE',  ( 4.904576926706878837, 5.977929128642318624, 18.88727191237769887 ) ) ;
#14652 = DIRECTION ( 'NONE',  ( -8.018662683283438208E-16, 5.975035461963189015E-16, 1.000000000000000000 ) ) ;
#14653 =( BOUNDED_CURVE ( )  B_SPLINE_CURVE ( 3, ( #11234, #4045, #7624, #8851 ),
 .UNSPECIFIED., .F., .T. ) 
 B_SPLINE_CURVE_WITH_KNOTS ( ( 4, 4 ),
 ( 3.141592653589793116, 4.400121501412645131 ),
 .UNSPECIFIED. ) 
 CURVE ( )  GEOMETRIC_REPRESENTATION_ITEM ( )  RATIONAL_B_SPLINE_CURVE ( ( 1.000000000000000000, 0.8723071003127529366, 0.8723071003127529366, 1.000000000000000000 ) ) 
 REPRESENTATION_ITEM ( '' )  );
#14654 = CARTESIAN_POINT ( 'NONE',  ( 16.55265521278991869, -23.76699243818182339, 4.741285470919336831 ) ) ;
#14655 = DIRECTION ( 'NONE',  ( -0.9988970074402869770, 0.04695496274984588270, -8.290375725550417844E-16 ) ) ;
#14656 = ADVANCED_FACE ( 'NONE', ( #4172 ), #731, .T. ) ;
#14657 = CARTESIAN_POINT ( 'NONE',  ( -13.01672903104007872, -13.79867928167105440, 51.25231026484399166 ) ) ;
#14658 = ORIENTED_EDGE ( 'NONE', *, *, #14030, .T. ) ;
#14659 = CARTESIAN_POINT ( 'NONE',  ( -15.42469986081099442, -23.50737899243800300, 56.85231026484400019 ) ) ;
#14660 = LINE ( 'NONE', #6381, #9497 ) ;
#14661 = VERTEX_POINT ( 'NONE', #9907 ) ;
#14662 = DIRECTION ( 'NONE',  ( 8.018662683283438208E-16, -5.975035461963189015E-16, -1.000000000000000000 ) ) ;
#14663 = EDGE_CURVE ( 'NONE', #4618, #8805, #10661, .T. ) ;
#14664 = CIRCLE ( 'NONE', #2202, 37.50000000000000000 ) ;
#14665 = DIRECTION ( 'NONE',  ( 0.8543800322332385511, 0.5196486895212286683, 3.746065934159130275E-16 ) ) ;
#14666 = CARTESIAN_POINT ( 'NONE',  ( -23.37741044072812713, -11.73331557219068877, 56.85231026484398598 ) ) ;
#14667 = ORIENTED_EDGE ( 'NONE', *, *, #1617, .F. ) ;
#14668 = DIRECTION ( 'NONE',  ( 0.000000000000000000, 0.000000000000000000, 1.000000000000000000 ) ) ;
#14669 = DIRECTION ( 'NONE',  ( 0.8160499452489514693, 0.5779813897169900905, 3.090169943749478258E-16 ) ) ;
#14670 = ITEM_DEFINED_TRANSFORMATION ( 'NONE', 'NONE', #1684,  #6789 ) ;
#14671 = CARTESIAN_POINT ( 'NONE',  ( -7.499699427612009472, -49.00737706678066274, 19.48780283923079537 ) ) ;
#14672 = VECTOR ( 'NONE', #6953, 1000.000000000000000 ) ;
#14673 = PLANE ( 'NONE',  #6959 ) ;
#14674 = EDGE_CURVE ( 'NONE', #9110, #6974, #11716, .T. ) ;
#14675 = CARTESIAN_POINT ( 'NONE',  ( -21.79090396836353705, -19.33464257641254136, 56.85231026484398598 ) ) ;
#14676 = VERTEX_POINT ( 'NONE', #7750 ) ;
#14677 = DIRECTION ( 'NONE',  ( 1.000000000000000000, 3.700743415417188632E-16, 0.000000000000000000 ) ) ;
#14678 = EDGE_CURVE ( 'NONE', #3877, #2114, #12434, .T. ) ;
#14679 = DIRECTION ( 'NONE',  ( 1.000000000000000000, -1.291538348938060198E-32, 1.054621095516909827E-16 ) ) ;
#14680 = ADVANCED_FACE ( 'NONE', ( #12209 ), #1806, .F. ) ;
#14681 = ORIENTED_EDGE ( 'NONE', *, *, #2454, .F. ) ;
#14683 = ORIENTED_EDGE ( 'NONE', *, *, #7054, .F. ) ;
#14682 = DIRECTION ( 'NONE',  ( -1.000000000000000000, 1.291538348938060198E-32, -1.054621095516909827E-16 ) ) ;
#14684 = CARTESIAN_POINT ( 'NONE',  ( -15.49969986081099727, -36.50737899243799944, 2.502310264843996546 ) ) ;
#14685 = PLANE ( 'NONE',  #5336 ) ;
#14686 = ADVANCED_FACE ( 'NONE', ( #1648 ), #13443, .F. ) ;
#14687 = LINE ( 'NONE', #3054, #9341 ) ;
#14688 = CARTESIAN_POINT ( 'NONE',  ( -8.792249626181712685, -48.86814062846791984, 43.66295784926125378 ) ) ;
#14689 = PLANE ( 'NONE',  #2615 ) ;
#14690 = CARTESIAN_POINT ( 'NONE',  ( -15.49969986081099904, -44.50737899243799944, -109.5506571639849938 ) ) ;
#14691 = EDGE_CURVE ( 'NONE', #9086, #532, #8906, .T. ) ;
#14692 = CARTESIAN_POINT ( 'NONE',  ( -20.94048570341206883, -6.243833066724571168, 56.85231026484398598 ) ) ;
#14693 = PLANE ( 'NONE',  #12786 ) ;
#14694 = CARTESIAN_POINT ( 'NONE',  ( 17.24684023006172140, -30.18180943203350708, 42.48680623383349797 ) ) ;
#14695 = ORIENTED_EDGE ( 'NONE', *, *, #14799, .T. ) ;
#14696 = FACE_OUTER_BOUND ( 'NONE', #6142, .T. ) ;
#14698 = EDGE_LOOP ( 'NONE', ( #8306, #4014, #1438, #12016, #11752, #5309 ) ) ;
#14697 = CARTESIAN_POINT ( 'NONE',  ( -15.49968909271368211, -3.507379016232285096, 61.71092834827113194 ) ) ;
#14699 = ORIENTED_EDGE ( 'NONE', *, *, #12266, .T. ) ;
#14700 = CIRCLE ( 'NONE', #1758, 0.4500000000000011768 ) ;
#14701 = DIRECTION ( 'NONE',  ( -0.2536112499260171349, -0.9673062255102895524, 3.746065934159117949E-16 ) ) ;
#14703 = ORIENTED_EDGE ( 'NONE', *, *, #8932, .T. ) ;
#14702 = CARTESIAN_POINT ( 'NONE',  ( 1.947694826113897770, 9.133458655267698845, 16.68946746569451278 ) ) ;
#14704 = AXIS2_PLACEMENT_3D ( 'NONE', #8896, #7738, #2094 ) ;
#14705 = DIRECTION ( 'NONE',  ( -0.3956847857120157075, 0.9183863840214729901, -8.660254037844388394E-16 ) ) ;
#14706 = DIRECTION ( 'NONE',  ( 0.9547156899063180546, 0.2975196656470009415, 5.877852522924732759E-16 ) ) ;
#14707 = PRODUCT_RELATED_PRODUCT_CATEGORY ( 'part', '', ( #6764 ) ) ;
#14708 = EDGE_CURVE ( 'NONE', #14274, #10935, #14427, .T. ) ;
#14709 = DIRECTION ( 'NONE',  ( 0.9925461516413222052, -0.006378148623806976711, -0.1217023257055263735 ) ) ;
#14710 =( LENGTH_UNIT ( ) NAMED_UNIT ( * ) SI_UNIT ( .MILLI., .METRE. ) );
#14711 = VECTOR ( 'NONE', #1498, 1000.000000000000114 ) ;
#14712 = AXIS2_PLACEMENT_3D ( 'NONE', #6632, #3289, #9012 ) ;
#14713 = CARTESIAN_POINT ( 'NONE',  ( -14.61203582816999891, -108.0739631064533484, -6.614055049357309812 ) ) ;
#14714 = AXIS2_PLACEMENT_3D ( 'NONE', #12517, #4559, #6979 ) ;
#14715 = VECTOR ( 'NONE', #1759, 1000.000000000000000 ) ;
#14716 = LINE ( 'NONE', #566, #2476 ) ;
#14717 = ORIENTED_EDGE ( 'NONE', *, *, #13036, .T. ) ;
#14718 = VERTEX_POINT ( 'NONE', #13585 ) ;
#14719 = CARTESIAN_POINT ( 'NONE',  ( -23.42445533997705454, -9.084766574938008432, 56.85231026484398598 ) ) ;
#14720 = VERTEX_POINT ( 'NONE', #3094 ) ;
#14721 = ORIENTED_EDGE ( 'NONE', *, *, #4245, .F. ) ;
#14722 = DIRECTION ( 'NONE',  ( 0.000000000000000000, -1.000000000000000000, -1.224646799147350002E-16 ) ) ;
#14723 = VERTEX_POINT ( 'NONE', #13361 ) ;
#14724 = DIRECTION ( 'NONE',  ( 0.000000000000000000, 0.000000000000000000, 1.000000000000000000 ) ) ;
#14725 = AXIS2_PLACEMENT_3D ( 'NONE', #12890, #7048, #11727 ) ;
#14726 = EDGE_CURVE ( 'NONE', #609, #12884, #12211, .T. ) ;
#14727 = AXIS2_PLACEMENT_3D ( 'NONE', #10034, #7735, #12422 ) ;
#14728 = CARTESIAN_POINT ( 'NONE',  ( -20.52642601085533869, -22.12321610861327770, 56.85231026484398598 ) ) ;
#14729 = DIRECTION ( 'NONE',  ( 1.000000000000000000, -1.291538348938060198E-32, 1.054621095516909827E-16 ) ) ;
#14730 = DIRECTION ( 'NONE',  ( -7.070501591499390115E-17, 1.224646799147350002E-16, -1.000000000000000000 ) ) ;
#14731 = CARTESIAN_POINT ( 'NONE',  ( -15.49969986081099904, -27.00737899243799944, -5.497689735156000346 ) ) ;
#14733 = DIRECTION ( 'NONE',  ( 0.2536112499260171349, 0.9673062255102895524, -3.746065934159117949E-16 ) ) ;
#14732 = FACE_OUTER_BOUND ( 'NONE', #11643, .T. ) ;
#14734 = ORIENTED_EDGE ( 'NONE', *, *, #10394, .F. ) ;
#14735 = CARTESIAN_POINT ( 'NONE',  ( -20.61203582816999713, -107.1622034095870077, -6.087689735156005533 ) ) ;
#14736 = PLANE ( 'NONE',  #10223 ) ;
#14737 = ORIENTED_EDGE ( 'NONE', *, *, #267, .T. ) ;
#14738 = CARTESIAN_POINT ( 'NONE',  ( -14.11952815701478059, -21.46390939632912875, 56.85231026484400019 ) ) ;
#14739 = VECTOR ( 'NONE', #8181, 1000.000000000000000 ) ;
#14740 = AXIS2_PLACEMENT_3D ( 'NONE', #4499, #7070, #3345 ) ;
#14741 = CARTESIAN_POINT ( 'NONE',  ( -21.60512016940287339, -5.619130273271679243, 54.00231026484397745 ) ) ;
#14742 = CARTESIAN_POINT ( 'NONE',  ( -17.09996058126371565, -94.70595027845364200, -10.75094526697130703 ) ) ;
#14743 = EDGE_LOOP ( 'NONE', ( #12728, #3483, #930, #11082, #1812 ) ) ;
#14744 = FACE_OUTER_BOUND ( 'NONE', #13946, .T. ) ;
#14745 = EDGE_CURVE ( 'NONE', #5367, #6300, #8678, .T. ) ;
#14746 = DIRECTION ( 'NONE',  ( -0.9983330752162417054, -0.05771543059946733500, -7.660444431189781397E-16 ) ) ;
#14747 =( LENGTH_UNIT ( ) NAMED_UNIT ( * ) SI_UNIT ( .MILLI., .METRE. ) );
#14748 = AXIS2_PLACEMENT_3D ( 'NONE', #11541, #1061, #5720 ) ;
#14749 = ADVANCED_FACE ( 'NONE', ( #6373 ), #11060, .F. ) ;
#14750 = CARTESIAN_POINT ( 'NONE',  ( -7.705418609685459330, -48.24386234041415378, 21.32367631506333439 ) ) ;
#14751 = FACE_OUTER_BOUND ( 'NONE', #9375, .T. ) ;
#14752 = DIRECTION ( 'NONE',  ( -0.5104125104778984845, -0.8599296884906632021, 1.045284632676530333E-16 ) ) ;
#14753 = APPLICATION_CONTEXT ( 'automotive_design' ) ;
#14754 = ORIENTED_EDGE ( 'NONE', *, *, #1117, .F. ) ;
#14755 = CARTESIAN_POINT ( 'NONE',  ( -12.23206416678372932, -4.082773856353237640, 56.85231026484398598 ) ) ;
#14756 = VECTOR ( 'NONE', #9006, 1000.000000000000227 ) ;
#14757 = ORIENTED_EDGE ( 'NONE', *, *, #9640, .F. ) ;
#14759 = ORIENTED_EDGE ( 'NONE', *, *, #12561, .T. ) ;
#14758 = CARTESIAN_POINT ( 'NONE',  ( -31.79969986081099975, 11.99262100756199878, 32.26206422150099939 ) ) ;
#14760 = ORIENTED_EDGE ( 'NONE', *, *, #2978, .T. ) ;
#14761 = VECTOR ( 'NONE', #11718, 1000.000000000000000 ) ;
#14762 = DIRECTION ( 'NONE',  ( -0.6251242923673533403, -0.7805252200231684867, -3.489949670250098342E-17 ) ) ;
#14763 = CARTESIAN_POINT ( 'NONE',  ( -15.49969986081100082, -109.4746705577010744, -0.8002025553967917482 ) ) ;
#14764 = EDGE_CURVE ( 'NONE', #5306, #14217, #3946, .T. ) ;
#14765 = DIRECTION ( 'NONE',  ( -0.7953815700667045130, -0.6061090314441981430, -2.756373558170028881E-16 ) ) ;
#14766 = EDGE_CURVE ( 'NONE', #2942, #10974, #14133, .T. ) ;
#14767 = PLANE ( 'NONE',  #5247 ) ;
#14768 = VECTOR ( 'NONE', #12897, 1000.000000000000227 ) ;
#14769 = EDGE_CURVE ( 'NONE', #10220, #6353, #3169, .T. ) ;
#14770 = CARTESIAN_POINT ( 'NONE',  ( -7.561698276841002375, -7.413715827245769496, 60.86289348305165703 ) ) ;
#14771 = CARTESIAN_POINT ( 'NONE',  ( -23.45327702811275827, -7.487309620431346069, 57.00231026484397745 ) ) ;
#14772 = DIRECTION ( 'NONE',  ( 1.000000000000000000, 0.000000000000000000, 0.000000000000000000 ) ) ;
#14773 = EDGE_CURVE ( 'NONE', #15001, #7413, #5464, .T. ) ;
#14774 = DIRECTION ( 'NONE',  ( -0.1855175943453168941, -0.9826409426582662920, 4.383711467890769768E-16 ) ) ;
#14775 = CARTESIAN_POINT ( 'NONE',  ( -15.49969986081099904, -2.007378992438000331, 24.21206422150099513 ) ) ;
#14776 = ORIENTED_EDGE ( 'NONE', *, *, #2804, .F. ) ;
#14777 = ORIENTED_EDGE ( 'NONE', *, *, #5602, .T. ) ;
#14778 = ORIENTED_EDGE ( 'NONE', *, *, #5588, .T. ) ;
#14779 = CARTESIAN_POINT ( 'NONE',  ( -7.425287632467987287, -13.60480674405941492, 56.85231026484400019 ) ) ;
#14781 = ORIENTED_EDGE ( 'NONE', *, *, #2103, .F. ) ;
#14780 = DIRECTION ( 'NONE',  ( -8.018662683283438208E-16, 5.975035461963189015E-16, 1.000000000000000000 ) ) ;
#14782 = DIRECTION ( 'NONE',  ( 0.000000000000000000, 0.000000000000000000, 1.000000000000000000 ) ) ;
#14783 = EDGE_CURVE ( 'NONE', #11671, #855, #253, .T. ) ;
#14784 = EDGE_CURVE ( 'NONE', #10153, #5382, #7900, .T. ) ;
#14785 = DIRECTION ( 'NONE',  ( 0.000000000000000000, 0.1872998510044689147, 0.9823027872370635460 ) ) ;
#14786 = SHAPE_REPRESENTATION_RELATIONSHIP ( 'NONE' , 'NONE' ,  #3931, #3153 ) ;
#14787 = CARTESIAN_POINT ( 'NONE',  ( -24.06473463808513813, -13.92741382918746496, 57.00231026484397745 ) ) ;
#14788 = CARTESIAN_POINT ( 'NONE',  ( -12.25471857405102405, -7.219983152459794162, 57.00231026484397745 ) ) ;
#14789 = ORIENTED_EDGE ( 'NONE', *, *, #10546, .T. ) ;
#14790 = CARTESIAN_POINT ( 'NONE',  ( 17.25200030867059553, -23.81382647575409806, 42.48144389911218610 ) ) ;
#14791 = ORIENTED_EDGE ( 'NONE', *, *, #2614, .T. ) ;
#14792 = DIRECTION ( 'NONE',  ( 0.5975035461963188466, 0.8018662683283437342, 0.000000000000000000 ) ) ;
#14793 = ORIENTED_EDGE ( 'NONE', *, *, #11585, .F. ) ;
#14794 = ORIENTED_EDGE ( 'NONE', *, *, #6626, .T. ) ;
#14795 = FACE_OUTER_BOUND ( 'NONE', #3906, .T. ) ;
#14796 = ORIENTED_EDGE ( 'NONE', *, *, #14024, .F. ) ;
#14797 = DIRECTION ( 'NONE',  ( 0.1165201156931293391, 0.9931883319083343320, -4.999999999999998416E-16 ) ) ;
#14798 = DIRECTION ( 'NONE',  ( 1.050965490997518184E-15, -0.05233595624294409832, -0.9986295347545739443 ) ) ;
#14799 = EDGE_CURVE ( 'NONE', #1039, #10194, #1031, .T. ) ;
#14800 = CARTESIAN_POINT ( 'NONE',  ( -15.49969986081095996, -67.00737899243799234, -5.497689735156000346 ) ) ;
#14801 = AXIS2_PLACEMENT_3D ( 'NONE', #9075, #12767, #8071 ) ;
#14802 = CARTESIAN_POINT ( 'NONE',  ( -10.27295246487022240, -6.088325032597582620, 56.85231026484398598 ) ) ;
#14803 = LINE ( 'NONE', #12438, #1561 ) ;
#14805 = DIRECTION ( 'NONE',  ( 0.000000000000000000, 0.1872998510044689147, 0.9823027872370635460 ) ) ;
#14804 = FACE_OUTER_BOUND ( 'NONE', #1464, .T. ) ;
#14806 = ORIENTED_EDGE ( 'NONE', *, *, #6991, .T. ) ;
#14807 = CARTESIAN_POINT ( 'NONE',  ( -7.886584594865180264, -46.96511696614940234, -3.039951761444701361 ) ) ;
#14808 = FACE_OUTER_BOUND ( 'NONE', #1984, .T. ) ;
#14809 = EDGE_CURVE ( 'NONE', #4418, #14123, #13885, .T. ) ;
#14810 = ORIENTED_EDGE ( 'NONE', *, *, #55, .F. ) ;
#14811 = ORIENTED_EDGE ( 'NONE', *, *, #8260, .F. ) ;
#14812 = CARTESIAN_POINT ( 'NONE',  ( -22.64353467404651354, -6.545608444567306172, 57.00231026484397745 ) ) ;
#14813 = EDGE_CURVE ( 'NONE', #9717, #13190, #6337, .T. ) ;
#14814 = FACE_OUTER_BOUND ( 'NONE', #1676, .T. ) ;
#14815 = AXIS2_PLACEMENT_3D ( 'NONE', #14690, #8870, #3057 ) ;
#14816 = ORIENTED_EDGE ( 'NONE', *, *, #4070, .T. ) ;
#14817 = CARTESIAN_POINT ( 'NONE',  ( 4.000300139189000959, -20.37340439622240851, 51.53354502093799994 ) ) ;
#14818 = DIRECTION ( 'NONE',  ( -0.03489949670250103858, 0.9993908270190956511, -3.489949670250003432E-17 ) ) ;
#14819 = APPLICATION_PROTOCOL_DEFINITION ( 'draft international standard', 'automotive_design', 1998, #10258 ) ;
#14820 = CARTESIAN_POINT ( 'NONE',  ( -7.649802761028805520, -48.47628348355012662, 21.04316911978840210 ) ) ;
#14821 = AXIS2_PLACEMENT_3D ( 'NONE', #2297, #5869, #9244 ) ;
#14822 = DIRECTION ( 'NONE',  ( 0.5975035461963188466, 0.8018662683283437342, 0.000000000000000000 ) ) ;
#14823 = DIRECTION ( 'NONE',  ( 0.2301973227387160703, -0.9731439732146149879, 7.660444431189776467E-16 ) ) ;
#14824 = ORIENTED_EDGE ( 'NONE', *, *, #7827, .F. ) ;
#14825 = CARTESIAN_POINT ( 'NONE',  ( -15.05574454978227550, -94.23694090986742822, -0.1444574119560445569 ) ) ;
#14826 = CARTESIAN_POINT ( 'NONE',  ( -21.60512016940287694, -5.619130273271677467, 57.00231026484397745 ) ) ;
#14827 = VECTOR ( 'NONE', #500, 1000.000000000000000 ) ;
#14828 = EDGE_CURVE ( 'NONE', #1753, #2020, #10752, .T. ) ;
#14829 = VERTEX_POINT ( 'NONE', #10358 ) ;
#14831 = ORIENTED_EDGE ( 'NONE', *, *, #7673, .F. ) ;
#14830 = DIRECTION ( 'NONE',  ( 0.000000000000000000, 0.000000000000000000, 1.000000000000000000 ) ) ;
#14832 = ORIENTED_EDGE ( 'NONE', *, *, #391, .F. ) ;
#14833 = DIRECTION ( 'NONE',  ( 0.6859287159822015090, -0.7276687409742212953, 9.848077530122081084E-16 ) ) ;
#14834 = LINE ( 'NONE', #10241, #13879 ) ;
#14835 = CONICAL_SURFACE ( 'NONE', #1645, 1664.279482350500075, 1.029744258676650093 ) ;
#14836 = PLANE ( 'NONE',  #5182 ) ;
#14837 = DIRECTION ( 'NONE',  ( 0.000000000000000000, 0.000000000000000000, 1.000000000000000000 ) ) ;
#14838 = AXIS2_PLACEMENT_3D ( 'NONE', #13335, #7498, #1618 ) ;
#14839 = CARTESIAN_POINT ( 'NONE',  ( -12.04767799572592502, -20.80732214584531548, 57.00231026484399166 ) ) ;
#14840 = CARTESIAN_POINT ( 'NONE',  ( -15.49969986081092266, -107.6986194064928100, -1.942511738887820361 ) ) ;
#14841 = AXIS2_PLACEMENT_3D ( 'NONE', #1675, #8705, #4049 ) ;
#14842 = AXIS2_PLACEMENT_3D ( 'NONE', #2485, #14271, #3788 ) ;
#14843 = CARTESIAN_POINT ( 'NONE',  ( -38.44424205229172031, 4.142642748859736379, 22.58640670738479983 ) ) ;
#14844 = CARTESIAN_POINT ( 'NONE',  ( -18.48721759179250412, -17.51671033407995282, 45.50231026484398456 ) ) ;
#14845 = EDGE_CURVE ( 'NONE', #9275, #8949, #4476, .T. ) ;
#14846 = VECTOR ( 'NONE', #6375, 1000.000000000000000 ) ;
#14847 = ORIENTED_EDGE ( 'NONE', *, *, #9440, .F. ) ;
#14848 = CARTESIAN_POINT ( 'NONE',  ( 15.84747201894258772, -29.85305842324876835, 44.79472527846461816 ) ) ;
#14849 = VERTEX_POINT ( 'NONE', #3402 ) ;
#14850 = CARTESIAN_POINT ( 'NONE',  ( -10.22560374232860347, -19.62253721876480128, 57.00231026484399166 ) ) ;
#14852 = ORIENTED_EDGE ( 'NONE', *, *, #5698, .T. ) ;
#14851 = CARTESIAN_POINT ( 'NONE',  ( -22.79913995068414678, -6.663256836605895295, 60.99553151634774650 ) ) ;
#14853 = EDGE_LOOP ( 'NONE', ( #13565, #412, #12798, #2619 ) ) ;
#14854 = ADVANCED_FACE ( 'NONE', ( #8052 ), #14898, .T. ) ;
#14855 = DIRECTION ( 'NONE',  ( 8.018662683283438208E-16, -5.975035461963189015E-16, -1.000000000000000000 ) ) ;
#14856 = ORIENTED_EDGE ( 'NONE', *, *, #14691, .T. ) ;
#14857 = CARTESIAN_POINT ( 'NONE',  ( -9.989347722329673829, -46.50737899243799944, -5.497689735156000346 ) ) ;
#14858 = CARTESIAN_POINT ( 'NONE',  ( -20.87112600995946821, -106.3120414409460466, -5.423877709286933246 ) ) ;
#14859 =( NAMED_UNIT ( * ) SI_UNIT ( $, .STERADIAN. ) SOLID_ANGLE_UNIT ( ) );
#14860 = ORIENTED_EDGE ( 'NONE', *, *, #4614, .F. ) ;
#14861 = LINE ( 'NONE', #10186, #769 ) ;
#14862 = AXIS2_PLACEMENT_3D ( 'NONE', #10281, #6747, #10123 ) ;
#14863 = CARTESIAN_POINT ( 'NONE',  ( -19.50984199700181776, -51.43466821614173057, -17.78337838361071732 ) ) ;
#14864 = EDGE_CURVE ( 'NONE', #10177, #2863, #12960, .T. ) ;
#14865 = ORIENTED_EDGE ( 'NONE', *, *, #6700, .F. ) ;
#14866 = CARTESIAN_POINT ( 'NONE',  ( 18.29963344931381286, -25.27049385225708278, 40.45631929470508936 ) ) ;
#14867 = EDGE_CURVE ( 'NONE', #8690, #10111, #11582, .T. ) ;
#14868 = ORIENTED_EDGE ( 'NONE', *, *, #5821, .T. ) ;
#14869 = VECTOR ( 'NONE', #11914, 1000.000000000000000 ) ;
#14870 = DIRECTION ( 'NONE',  ( -0.9931883319083343320, 0.1165201156931293391, -8.660254037844386422E-16 ) ) ;
#14871 = ORIENTED_EDGE ( 'NONE', *, *, #14499, .F. ) ;
#14872 = ORIENTED_EDGE ( 'NONE', *, *, #2331, .T. ) ;
#14873 = EDGE_CURVE ( 'NONE', #8778, #3521, #5339, .T. ) ;
#14874 = CARTESIAN_POINT ( 'NONE',  ( -7.264457220180047692, -15.89840986842769333, 56.85231026484400019 ) ) ;
#14875 = EDGE_LOOP ( 'NONE', ( #3381, #2076, #13897, #4129 ) ) ;
#14876 = CARTESIAN_POINT ( 'NONE',  ( -8.572300031023576850, -40.49742984648624855, 56.35711988542138329 ) ) ;
#14877 =( BOUNDED_CURVE ( )  B_SPLINE_CURVE ( 3, ( #5392, #7822, #8682, #13364 ),
 .UNSPECIFIED., .F., .T. ) 
 B_SPLINE_CURVE_WITH_KNOTS ( ( 4, 4 ),
 ( 4.712388980384689674, 6.283185307179585344 ),
 .UNSPECIFIED. ) 
 CURVE ( )  GEOMETRIC_REPRESENTATION_ITEM ( )  RATIONAL_B_SPLINE_CURVE ( ( 1.000000000000000000, 0.8047378541243649375, 0.8047378541243649375, 1.000000000000000000 ) ) 
 REPRESENTATION_ITEM ( '' )  );
#14878 = CARTESIAN_POINT ( 'NONE',  ( -15.50552586659557797, -13.55703840903364288, 56.85231026484398598 ) ) ;
#14879 = LINE ( 'NONE', #14949, #9242 ) ;
#14880 = LINE ( 'NONE', #5466, #11927 ) ;
#14881 = DIRECTION ( 'NONE',  ( -1.000000000000000000, 1.291538348938060198E-32, -1.054621095516909827E-16 ) ) ;
#14883 = CARTESIAN_POINT ( 'NONE',  ( 6.590007710802169072, 5.168430268676311279, 28.44896274323930285 ) ) ;
#14882 = DIRECTION ( 'NONE',  ( 0.000000000000000000, -1.334178587669858246E-16, 1.000000000000000000 ) ) ;
#14884 = ORIENTED_EDGE ( 'NONE', *, *, #1101, .T. ) ;
#14885 = CARTESIAN_POINT ( 'NONE',  ( -8.992083836518995454, -50.38952316532486009, 0.3844544377308600214 ) ) ;
#14886 = EDGE_CURVE ( 'NONE', #1644, #1569, #14879, .T. ) ;
#14887 = VECTOR ( 'NONE', #295, 1000.000000000000114 ) ;
#14888 = DIRECTION ( 'NONE',  ( -0.8160499452489514693, -0.5779813897169900905, -3.090169943749478258E-16 ) ) ;
#14889 = ORIENTED_EDGE ( 'NONE', *, *, #743, .F. ) ;
#14890 = VERTEX_POINT ( 'NONE', #3173 ) ;
#14891 = DIRECTION ( 'NONE',  ( 0.000000000000000000, 0.1872998510044689147, 0.9823027872370635460 ) ) ;
#14892 = CARTESIAN_POINT ( 'NONE',  ( -17.06800750706793224, -36.64961894308596868, -17.96750743336168910 ) ) ;
#14893 = CARTESIAN_POINT ( 'NONE',  ( -18.04103863274072594, -14.60230930160663121, 51.00231026484399166 ) ) ;
#14894 = CARTESIAN_POINT ( 'NONE',  ( -19.06972223273333711, -21.85101071153832919, 57.00231026484399166 ) ) ;
#14895 = ORIENTED_EDGE ( 'NONE', *, *, #6607, .F. ) ;
#14896 = DIRECTION ( 'NONE',  ( 0.5975035461963190686, 0.8018662683283437342, 1.972152263052529514E-31 ) ) ;
#14897 = LINE ( 'NONE', #13901, #7061 ) ;
#14898 = CONICAL_SURFACE ( 'NONE', #13656, 19.00000000000000000, 1.047197551196598297 ) ;
#14899 = EDGE_CURVE ( 'NONE', #2017, #2175, #11209, .T. ) ;
#14900 = DIRECTION ( 'NONE',  ( 8.018662683283438208E-16, -5.975035461963189015E-16, -1.000000000000000000 ) ) ;
#14901 = CARTESIAN_POINT ( 'NONE',  ( -5.923714809816990723, -16.30043024566306187, 57.00231026484399166 ) ) ;
#14902 = DIRECTION ( 'NONE',  ( 0.3857661296576155308, 0.9225966037272105291, -2.419218955996680478E-16 ) ) ;
#14904 = VERTEX_POINT ( 'NONE', #9669 ) ;
#14903 = AXIS2_PLACEMENT_3D ( 'NONE', #8130, #12821, #6829 ) ;
#14905 = FACE_OUTER_BOUND ( 'NONE', #10842, .T. ) ;
#14906 = CARTESIAN_POINT ( 'NONE',  ( -21.45979773411919567, -21.50599501901345789, 51.00231026484399166 ) ) ;
#14907 = LINE ( 'NONE', #6776, #11828 ) ;
#14908 = ORIENTED_EDGE ( 'NONE', *, *, #5212, .F. ) ;
#14909 = CARTESIAN_POINT ( 'NONE',  ( -15.49969986081099904, 37.56536188261469533, 29.46206422150100579 ) ) ;
#14910 = VERTEX_POINT ( 'NONE', #14108 ) ;
#14911 = CARTESIAN_POINT ( 'NONE',  ( -20.31707134655588121, -4.772760685475331499, 54.00231026484397745 ) ) ;
#14912 = CARTESIAN_POINT ( 'NONE',  ( -11.97987666612771207, -20.77526002325937782, 56.85231026484400019 ) ) ;
#14913 = AXIS2_PLACEMENT_3D ( 'NONE', #13049, #11728, #3703 ) ;
#14914 = PLANE ( 'NONE',  #68 ) ;
#14915 = CARTESIAN_POINT ( 'NONE',  ( -8.659108278886616716, -48.65678357935241394, 43.21545986666426842 ) ) ;
#14916 = EDGE_CURVE ( 'NONE', #12154, #14904, #11887, .T. ) ;
#14917 = DIRECTION ( 'NONE',  ( -0.8543800322332379960, -0.5196486895212294455, -3.746065934159121401E-16 ) ) ;
#14918 = CARTESIAN_POINT ( 'NONE',  ( -15.19697172008446096, -10.92700001391350284, 51.00231026484399166 ) ) ;
#14919 = DIRECTION ( 'NONE',  ( -8.018662683283438208E-16, 5.975035461963189015E-16, 1.000000000000000000 ) ) ;
#14920 = CARTESIAN_POINT ( 'NONE',  ( -31.89126067837590028, -25.75737899243799944, -17.99768973515599768 ) ) ;
#14921 = ORIENTED_EDGE ( 'NONE', *, *, #13085, .T. ) ;
#14922 = DIRECTION ( 'NONE',  ( 0.000000000000000000, 1.239088197126290817E-16, -1.000000000000000000 ) ) ;
#14923 = ORIENTED_EDGE ( 'NONE', *, *, #9513, .T. ) ;
#14925 = VERTEX_POINT ( 'NONE', #121 ) ;
#14924 = PLANE ( 'NONE',  #5930 ) ;
#14926 = EDGE_LOOP ( 'NONE', ( #2883, #13136, #7890, #4557 ) ) ;
#14927 = CARTESIAN_POINT ( 'NONE',  ( -18.09969986081100402, -109.0157871265392799, -1.700811998197179431 ) ) ;
#14928 = ORIENTED_EDGE ( 'NONE', *, *, #12178, .F. ) ;
#14929 = LINE ( 'NONE', #13635, #13200 ) ;
#14930 = AXIS2_PLACEMENT_3D ( 'NONE', #10110, #14637, #13348 ) ;
#14931 = EDGE_CURVE ( 'NONE', #10921, #3108, #4932, .T. ) ;
#14932 = DIRECTION ( 'NONE',  ( -0.6334982226805353500, 0.7737441449604661736, -9.702957262759963093E-16 ) ) ;
#14933 = EDGE_CURVE ( 'NONE', #5527, #3941, #1410, .T. ) ;
#14934 = EDGE_LOOP ( 'NONE', ( #3391, #6837, #3224, #10713 ) ) ;
#14935 = CARTESIAN_POINT ( 'NONE',  ( -16.55482201156862487, -52.45476196004928227, -17.98636559174942562 ) ) ;
#14936 = ORIENTED_EDGE ( 'NONE', *, *, #12891, .F. ) ;
#14937 = DIRECTION ( 'NONE',  ( 0.000000000000000000, 0.000000000000000000, 1.000000000000000000 ) ) ;
#14938 = ORIENTED_EDGE ( 'NONE', *, *, #11807, .T. ) ;
#14939 = DIRECTION ( 'NONE',  ( -0.9085715390340231012, 0.4177292884839972076, -9.781476007338054812E-16 ) ) ;
#14940 = ORIENTED_EDGE ( 'NONE', *, *, #10357, .F. ) ;
#14941 = VERTEX_POINT ( 'NONE', #10742 ) ;
#14942 = AXIS2_PLACEMENT_3D ( 'NONE', #11624, #14004, #7179 ) ;
#14943 = DIRECTION ( 'NONE',  ( 0.000000000000000000, -1.850371707708594316E-16, 1.000000000000000000 ) ) ;
#14944 = ORIENTED_EDGE ( 'NONE', *, *, #590, .F. ) ;
#14945 = CARTESIAN_POINT ( 'NONE',  ( -8.995873580312741424, -39.84177233736869539, 56.43429974597158605 ) ) ;
#14946 = ADVANCED_FACE ( 'NONE', ( #7359 ), #6132, .F. ) ;
#14947 = CARTESIAN_POINT ( 'NONE',  ( -15.49969986081100259, -19.50737899243800300, -17.99768973515599768 ) ) ;
#14948 = AXIS2_PLACEMENT_3D ( 'NONE', #12203, #2865, #5097 ) ;
#14949 = CARTESIAN_POINT ( 'NONE',  ( -31.79969986081099975, 20.99262100756200056, 24.21206422150099868 ) ) ;
#14950 = EDGE_CURVE ( 'NONE', #10777, #6540, #3389, .T. ) ;
#14951 = TOROIDAL_SURFACE ( 'NONE', #14714, 1.600000000000000089, 0.1499999999999999944 ) ;
#14952 = AXIS2_PLACEMENT_3D ( 'NONE', #6175, #385, #5042 ) ;
#14953 = EDGE_CURVE ( 'NONE', #6669, #11993, #12184, .T. ) ;
#14954 = B_SPLINE_CURVE_WITH_KNOTS ( 'NONE', 3,
 ( #1956, #11282, #732, #810 ),
 .UNSPECIFIED., .F., .F.,
 ( 4, 4 ),
 ( 0.01169941957287879905, 0.01381006638855979997 ),
 .UNSPECIFIED. ) ;
#14955 = FACE_OUTER_BOUND ( 'NONE', #4133, .T. ) ;
#14957 = CARTESIAN_POINT ( 'NONE',  ( -15.61203582817000246, -106.3249253597797406, -5.117531130952053253 ) ) ;
#14956 = PLANE ( 'NONE',  #13497 ) ;
#14958 = ORIENTED_EDGE ( 'NONE', *, *, #8696, .F. ) ;
#14959 = DIRECTION ( 'NONE',  ( 1.000000000000000000, 1.201369187114119994E-15, 9.616040805000176517E-16 ) ) ;
#14960 = CARTESIAN_POINT ( 'NONE',  ( -18.24645429046799450, -17.08409997186676321, -13.18801804347263129 ) ) ;
#14961 = ORIENTED_EDGE ( 'NONE', *, *, #1554, .T. ) ;
#14962 = ADVANCED_FACE ( 'NONE', ( #8284 ), #3782, .F. ) ;
#14963 = ORIENTED_EDGE ( 'NONE', *, *, #2541, .F. ) ;
#14964 = CARTESIAN_POINT ( 'NONE',  ( -23.08905235891587182, -41.92403831085029964, -17.22224902766740584 ) ) ;
#14965 = CIRCLE ( 'NONE', #4210, 0.4500000000000011768 ) ;
#14966 = ORIENTED_EDGE ( 'NONE', *, *, #8456, .F. ) ;
#14967 = CARTESIAN_POINT ( 'NONE',  ( -15.42469986081099442, -26.50737899243800300, 56.85231026484400019 ) ) ;
#14968 = AXIS2_PLACEMENT_3D ( 'NONE', #13159, #6171, #1820 ) ;
#14969 = VECTOR ( 'NONE', #2397, 1000.000000000000000 ) ;
#14970 = LINE ( 'NONE', #1197, #5359 ) ;
#14971 = EDGE_CURVE ( 'NONE', #6233, #6222, #6302, .T. ) ;
#14972 = CARTESIAN_POINT ( 'NONE',  ( -7.734307812155742923, -7.246443652516327383, 57.00231026484399166 ) ) ;
#14973 = VECTOR ( 'NONE', #12332, 1000.000000000000000 ) ;
#14974 = DIRECTION ( 'NONE',  ( 1.000000000000000000, 1.201369187114119994E-15, 9.616040805000176517E-16 ) ) ;
#14975 = FACE_OUTER_BOUND ( 'NONE', #6668, .T. ) ;
#14976 = ORIENTED_EDGE ( 'NONE', *, *, #12641, .T. ) ;
#14977 = DIRECTION ( 'NONE',  ( -8.018662683283438208E-16, 5.975035461963189015E-16, 1.000000000000000000 ) ) ;
#14978 = DIRECTION ( 'NONE',  ( -8.018662683283438208E-16, 5.975035461963189015E-16, 1.000000000000000000 ) ) ;
#14979 = FACE_OUTER_BOUND ( 'NONE', #6049, .T. ) ;
#14980 = LINE ( 'NONE', #4505, #8025 ) ;
#14981 = EDGE_LOOP ( 'NONE', ( #172, #6895, #12516, #9868 ) ) ;
#14982 = FACE_OUTER_BOUND ( 'NONE', #1497, .T. ) ;
#14983 = ORIENTED_EDGE ( 'NONE', *, *, #14886, .T. ) ;
#14984 = ADVANCED_FACE ( 'NONE', ( #5011, #14339 ), #9515, .T. ) ;
#14985 = CARTESIAN_POINT ( 'NONE',  ( -15.49969986081091200, -13.50737899243823215, 48.00231026484398456 ) ) ;
#14986 = CARTESIAN_POINT ( 'NONE',  ( -22.53804163936502647, -6.438972523632137346, 54.00231026484397745 ) ) ;
#14987 = AXIS2_PLACEMENT_3D ( 'NONE', #8164, #11688, #10693 ) ;
#14989 = VECTOR ( 'NONE', #13811, 1000.000000000000000 ) ;
#14988 = CARTESIAN_POINT ( 'NONE',  ( -15.49969986081099904, 9.919219809770899232, 24.21206422150099868 ) ) ;
#14990 = DIRECTION ( 'NONE',  ( -8.018662683283438208E-16, 5.975035461963189015E-16, 1.000000000000000000 ) ) ;
#14991 = CARTESIAN_POINT ( 'NONE',  ( -7.173558800825103887, -7.936225612681747421, 60.77745208716326886 ) ) ;
#14992 = DIRECTION ( 'NONE',  ( 0.000000000000000000, 1.000000000000000000, 1.224646799147350002E-16 ) ) ;
#14993 = CARTESIAN_POINT ( 'NONE',  ( -35.18004919290292776, -38.26834254388187162, 51.42305902976909948 ) ) ;
#14994 = DIRECTION ( 'NONE',  ( -8.018662683283438208E-16, 5.975035461963189015E-16, 1.000000000000000000 ) ) ;
#14995 = ORIENTED_EDGE ( 'NONE', *, *, #1554, .F. ) ;
#14996 = DIRECTION ( 'NONE',  ( -0.5975035461963217331, -0.8018662683283416248, 0.000000000000000000 ) ) ;
#14997 = ORIENTED_EDGE ( 'NONE', *, *, #8139, .T. ) ;
#14999 = ORIENTED_EDGE ( 'NONE', *, *, #9140, .F. ) ;
#14998 = DIRECTION ( 'NONE',  ( 0.6519834208811541298, 0.7582332219680880669, 6.975647374412577675E-17 ) ) ;
#15000 = ADVANCED_FACE ( 'NONE', ( #2633 ), #8515, .F. ) ;
#15001 = VERTEX_POINT ( 'NONE', #12343 ) ;
#15002 = EDGE_CURVE ( 'NONE', #1247, #4771, #945, .T. ) ;
#15003 = DIRECTION ( 'NONE',  ( 0.000000000000000000, -1.000000000000000000, -1.224646799147350002E-16 ) ) ;
#15004 = ORIENTED_EDGE ( 'NONE', *, *, #11324, .T. ) ;
#15005 = VECTOR ( 'NONE', #4161, 1000.000000000000114 ) ;
#15006 = DIRECTION ( 'NONE',  ( 0.5975035461963188466, 0.8018662683283437342, 0.000000000000000000 ) ) ;
#15007 = AXIS2_PLACEMENT_3D ( 'NONE', #7925, #2125, #9304 ) ;
#15008 = CARTESIAN_POINT ( 'NONE',  ( -20.85369739404940148, -106.8082859091853862, -5.057075470912998583 ) ) ;
#15009 = VERTEX_POINT ( 'NONE', #12191 ) ;
#15010 = CARTESIAN_POINT ( 'NONE',  ( -22.42809723928562349, -48.51567270060554193, -17.35231326048090850 ) ) ;
#15011 = B_SPLINE_CURVE_WITH_KNOTS ( 'NONE', 3,
 ( #1854, #6500, #10100, #11261, #10026, #13217, #14702, #4228, #8882, #781, #13564, #365 ),
 .UNSPECIFIED., .F., .F.,
 ( 4, 2, 2, 2, 2, 4 ),
 ( 0.000000000000000000, 0.2500000000000018874, 0.3750000000000034972, 0.4375000000000036637, 0.5000000000000037748, 1.000000000000000000 ),
 .UNSPECIFIED. ) ;
#15012 = ORIENTED_EDGE ( 'NONE', *, *, #5891, .T. ) ;
#15013 = CARTESIAN_POINT ( 'NONE',  ( -24.36945568363038461, -11.58678490633884373, 57.00231026484397745 ) ) ;
#15014 = VERTEX_POINT ( 'NONE', #5149 ) ;
#15015 = DIRECTION ( 'NONE',  ( 8.018662683283438208E-16, -5.975035461963189015E-16, -1.000000000000000000 ) ) ;
#15016 = ORIENTED_EDGE ( 'NONE', *, *, #15040, .T. ) ;
#15017 = VERTEX_POINT ( 'NONE', #6506 ) ;
#15018 = DIRECTION ( 'NONE',  ( -0.7737441449604673949, -0.6334982226805337957, -2.419218955996708581E-16 ) ) ;
#15019 = STYLED_ITEM ( 'NONE', ( #11654 ), #7461 ) ;
#15020 = EDGE_CURVE ( 'NONE', #13245, #4959, #3629, .T. ) ;
#15021 = LINE ( 'NONE', #12429, #3719 ) ;
#15022 = VERTEX_POINT ( 'NONE', #2850 ) ;
#15023 = CARTESIAN_POINT ( 'NONE',  ( -22.51561314124201374, -20.67385552401155380, 56.34133000697264748 ) ) ;
#15024 = FILL_AREA_STYLE ('',( #2332 ) ) ;
#15025 = CARTESIAN_POINT ( 'NONE',  ( -15.61203582817000068, -106.1798807882712765, -5.562105325730671623 ) ) ;
#15026 = AXIS2_PLACEMENT_3D ( 'NONE', #13006, #14067, #4895 ) ;
#15027 = CARTESIAN_POINT ( 'NONE',  ( -7.527662185239785586, -45.17397162665944421, 21.61993551438897754 ) ) ;
#15029 = LINE ( 'NONE', #2261, #5807 ) ;
#15028 = DIRECTION ( 'NONE',  ( 0.9320450512859435044, -0.1973458207444490908, -0.3038859151196102726 ) ) ;
#15030 = VERTEX_POINT ( 'NONE', #8812 ) ;
#15031 = FACE_OUTER_BOUND ( 'NONE', #2424, .T. ) ;
#15032 = CARTESIAN_POINT ( 'NONE',  ( -18.47295845456654106, -16.89792307448851005, -13.17045985127346341 ) ) ;
#15033 = VERTEX_POINT ( 'NONE', #7438 ) ;
#15034 = VERTEX_POINT ( 'NONE', #3076 ) ;
#15035 = LINE ( 'NONE', #3265, #2257 ) ;
#15036 = EDGE_CURVE ( 'NONE', #5221, #3880, #2934, .T. ) ;
#15037 = CARTESIAN_POINT ( 'NONE',  ( -23.44892144575882043, -43.46354585320516151, -17.14562330798139200 ) ) ;
#15038 = ORIENTED_EDGE ( 'NONE', *, *, #3088, .F. ) ;
#15039 = LINE ( 'NONE', #5777, #3206 ) ;
#15040 = EDGE_CURVE ( 'NONE', #7558, #8222, #12268, .T. ) ;
#15041 = AXIS2_PLACEMENT_3D ( 'NONE', #11832, #14430, #10910 ) ;
#15042 = LINE ( 'NONE', #6917, #12701 ) ;
#15043 = EDGE_CURVE ( 'NONE', #13555, #7254, #9816, .T. ) ;
#15044 = CARTESIAN_POINT ( 'NONE',  ( -8.791486474964742115, -6.124933722071904896, 56.85231026484398598 ) ) ;
#15045 = DIRECTION ( 'NONE',  ( -8.018662683283438208E-16, 5.975035461963189015E-16, 1.000000000000000000 ) ) ;
#15046 = FACE_OUTER_BOUND ( 'NONE', #6032, .T. ) ;
#15047 = ORIENTED_EDGE ( 'NONE', *, *, #7381, .T. ) ;
#15048 = CARTESIAN_POINT ( 'NONE',  ( -13.02077215656149889, -91.65099479865030219, -0.7314108185287553354 ) ) ;
#15049 = CIRCLE ( 'NONE', #9438, 0.2000000000000012046 ) ;
#15050 = DIRECTION ( 'NONE',  ( 0.5975035461963189576, 0.8018662683283437342, 0.000000000000000000 ) ) ;
#15051 = DIRECTION ( 'NONE',  ( -1.767853594929135667E-17, -0.9895257890689693747, -0.1443562010009731278 ) ) ;
#15052 = EDGE_CURVE ( 'NONE', #6890, #11369, #1560, .T. ) ;
#15053 = B_SPLINE_CURVE_WITH_KNOTS ( 'NONE', 3,
 ( #12904, #2265, #2113, #2188, #10289, #6976, #6756, #14960, #15032, #7910, #4636, #47, #11737, #7982, #13891, #1259, #11439, #12599 ),
 .UNSPECIFIED., .F., .F.,
 ( 4, 2, 2, 2, 2, 2, 2, 2, 4 ),
 ( 0.02128456778516834430, 0.02217184244320109451, 0.02305911710123384473, 0.02394639175926659494, 0.02483366641729934515, 0.02572094107533209884, 0.02660821573336484905, 0.02749549039139759926, 0.02838276504943034947 ),
 .UNSPECIFIED. ) ;
#15055 = EDGE_CURVE ( 'NONE', #3406, #3165, #11195, .T. ) ;
#15054 = CARTESIAN_POINT ( 'NONE',  ( -20.06719866676104402, -21.34952185377683165, 56.85231026484398598 ) ) ;
#15056 = VERTEX_POINT ( 'NONE', #14560 ) ;
#15057 = FACE_OUTER_BOUND ( 'NONE', #11465, .T. ) ;
#15058 = ORIENTED_EDGE ( 'NONE', *, *, #14592, .F. ) ;
#15059 = EDGE_CURVE ( 'NONE', #9104, #3051, #2783, .T. ) ;
#15060 = DIRECTION ( 'NONE',  ( -0.5491495666976170531, 0.8357240892757724637, -9.396926207859082113E-16 ) ) ;
#15061 = DIRECTION ( 'NONE',  ( 0.5975035461963189576, 0.8018662683283437342, 0.000000000000000000 ) ) ;
#15062 = DIRECTION ( 'NONE',  ( 0.000000000000000000, 1.000000000000000000, 1.224646799147350002E-16 ) ) ;
#15063 = AXIS2_PLACEMENT_3D ( 'NONE', #12230, #4973, #14445 ) ;
#15064 = FACE_OUTER_BOUND ( 'NONE', #4791, .T. ) ;
#15065 = VECTOR ( 'NONE', #4313, 1000.000000000000114 ) ;
#15066 = DIRECTION ( 'NONE',  ( 0.000000000000000000, 1.000000000000000000, 1.224646799147350002E-16 ) ) ;
#15067 = CARTESIAN_POINT ( 'NONE',  ( -20.60655739512266749, -107.1622034095862972, -7.162689735156005710 ) ) ;
#15068 = DIRECTION ( 'NONE',  ( -8.018662683283438208E-16, 5.975035461963189015E-16, 1.000000000000000000 ) ) ;
#15069 = ORIENTED_EDGE ( 'NONE', *, *, #12529, .F. ) ;
#15070 = CARTESIAN_POINT ( 'NONE',  ( -15.49969986081092088, -13.50737899243822504, 57.00231026484397745 ) ) ;
#15071 = VECTOR ( 'NONE', #3275, 999.9999999999998863 ) ;
#15072 = EDGE_CURVE ( 'NONE', #6605, #10753, #7661, .T. ) ;
#15073 = ORIENTED_EDGE ( 'NONE', *, *, #13765, .F. ) ;
#15075 = ORIENTED_EDGE ( 'NONE', *, *, #4592, .T. ) ;
#15074 = DIRECTION ( 'NONE',  ( 1.000000000000000000, 0.000000000000000000, 0.000000000000000000 ) ) ;
#15076 = ORIENTED_EDGE ( 'NONE', *, *, #13137, .F. ) ;
#15077 = EDGE_CURVE ( 'NONE', #3452, #13179, #11116, .T. ) ;
#15078 = DIRECTION ( 'NONE',  ( 0.000000000000000000, 2.220446049250313081E-16, -1.000000000000000000 ) ) ;
#15079 = ORIENTED_EDGE ( 'NONE', *, *, #7017, .T. ) ;
#15080 = LINE ( 'NONE', #1931, #11230 ) ;
#15081 = CARTESIAN_POINT ( 'NONE',  ( -6.426265323245524463, -13.69186664111786200, 56.85231026484400019 ) ) ;
#15082 = PLANE ( 'NONE',  #982 ) ;
#15083 = VECTOR ( 'NONE', #63, 1000.000000000000227 ) ;
#15084 = EDGE_CURVE ( 'NONE', #858, #15022, #7514, .T. ) ;
#15085 = VECTOR ( 'NONE', #14701, 1000.000000000000227 ) ;
#15086 = CARTESIAN_POINT ( 'NONE',  ( -20.16554002329735340, -51.01103853986323600, -17.70692683075240126 ) ) ;
#15087 = VERTEX_POINT ( 'NONE', #9891 ) ;
#15088 = CARTESIAN_POINT ( 'NONE',  ( -13.50483658114444552, -17.55182216082192781, -13.23583201258599296 ) ) ;
#15089 = ORIENTED_EDGE ( 'NONE', *, *, #8847, .T. ) ;
#15090 = CARTESIAN_POINT ( 'NONE',  ( -15.49969986081099371, -32.00737899243799234, -13.28793577849899599 ) ) ;
#15091 = ORIENTED_EDGE ( 'NONE', *, *, #8012, .T. ) ;
#15092 = ORIENTED_EDGE ( 'NONE', *, *, #11357, .T. ) ;
#15093 = DIRECTION ( 'NONE',  ( 0.000000000000000000, -1.000000000000000000, -1.224646799147350002E-16 ) ) ;
#15094 = ORIENTED_EDGE ( 'NONE', *, *, #11504, .F. ) ;
#15095 = AXIS2_PLACEMENT_3D ( 'NONE', #2186, #4409, #12598 ) ;
#15096 = CARTESIAN_POINT ( 'NONE',  ( -20.44297195033120929, -22.20066666004292699, 56.67562539687022394 ) ) ;
#15097 = VECTOR ( 'NONE', #14733, 1000.000000000000227 ) ;
#15098 = VECTOR ( 'NONE', #9799, 1000.000000000000114 ) ;
#15099 = FACE_OUTER_BOUND ( 'NONE', #3223, .T. ) ;
#15100 = CARTESIAN_POINT ( 'NONE',  ( -10.12854551587539298, -90.53879060557073899, -5.553494450699679064 ) ) ;
#15101 = ADVANCED_FACE ( 'NONE', ( #5083 ), #5299, .F. ) ;
#15102 = CARTESIAN_POINT ( 'NONE',  ( -7.705950972875354132, -46.29720360269725177, 21.99401816995757386 ) ) ;
#15104 = DIRECTION ( 'NONE',  ( -8.018662683283438208E-16, 5.975035461963189015E-16, 1.000000000000000000 ) ) ;
#15103 = DIRECTION ( 'NONE',  ( -0.3190779711151160991, -0.04960027561187737438, -0.9464296386991939425 ) ) ;
#15105 = ORIENTED_EDGE ( 'NONE', *, *, #531, .F. ) ;
#15106 = CARTESIAN_POINT ( 'NONE',  ( -7.502323095902962535, -44.76088757143082830, 42.70304391562847002 ) ) ;
#15107 = DIRECTION ( 'NONE',  ( 8.018662683283438208E-16, -5.975035461963189015E-16, -1.000000000000000000 ) ) ;
#15108 = ORIENTED_EDGE ( 'NONE', *, *, #6700, .T. ) ;
#15109 = ORIENTED_EDGE ( 'NONE', *, *, #5100, .F. ) ;
#15110 = PLANE ( 'NONE',  #14477 ) ;
#15111 = CARTESIAN_POINT ( 'NONE',  ( -15.21745595230144232, -22.57829892241827352, 57.00231026484399166 ) ) ;
#15112 = EDGE_LOOP ( 'NONE', ( #14721, #3244, #5021, #277 ) ) ;
#15113 = CARTESIAN_POINT ( 'NONE',  ( -13.41639018438039699, -15.05973874201012741, 51.00231026484399166 ) ) ;
#15114 = ORIENTED_EDGE ( 'NONE', *, *, #3830, .F. ) ;
#15115 = DIRECTION ( 'NONE',  ( -0.9578660637129379207, 0.2872152572324145892, -9.396926207859088029E-16 ) ) ;
#15116 = LINE ( 'NONE', #3492, #1462 ) ;
#15117 = EDGE_CURVE ( 'NONE', #2422, #2471, #3930, .T. ) ;
#15118 = DIRECTION ( 'NONE',  ( 0.000000000000000000, 0.1872998510044759646, 0.9823027872370621028 ) ) ;
#15119 = CIRCLE ( 'NONE', #3401, 9.974999999999999645 ) ;
#15120 = AXIS2_PLACEMENT_3D ( 'NONE', #8423, #8190, #9420 ) ;
#15121 = DIRECTION ( 'NONE',  ( -0.8357240892757725748, -0.5491495666976171641, -3.420201433256691137E-16 ) ) ;
#15122 = DIRECTION ( 'NONE',  ( 8.018662683283438208E-16, -5.975035461963189015E-16, -1.000000000000000000 ) ) ;
#15123 = ADVANCED_FACE ( 'NONE', ( #712 ), #5374, .T. ) ;
#15124 = EDGE_LOOP ( 'NONE', ( #10597, #14976, #2761, #1832 ) ) ;
#15125 = CARTESIAN_POINT ( 'NONE',  ( -15.49969986081092088, -13.50737899243822504, 57.00231026484397745 ) ) ;
#15126 = NEXT_ASSEMBLY_USAGE_OCCURRENCE ( 'NAUO1', ' ', ' ', #9279, #11525, $ ) ;
#15127 = NEXT_ASSEMBLY_USAGE_OCCURRENCE ( 'NAUO2', ' ', ' ', #9279, #9473, $ ) ;
#15128 = NEXT_ASSEMBLY_USAGE_OCCURRENCE ( 'NAUO3', ' ', ' ', #9279, #7495, $ ) ;
#15129 = NEXT_ASSEMBLY_USAGE_OCCURRENCE ( 'NAUO4', ' ', ' ', #9279, #12004, $ ) ;
#15130 = NEXT_ASSEMBLY_USAGE_OCCURRENCE ( 'NAUO5', ' ', ' ', #9279, #10680, $ ) ;
#15131 = NEXT_ASSEMBLY_USAGE_OCCURRENCE ( 'NAUO6', ' ', ' ', #9279, #14249, $ ) ;
#15132 = NEXT_ASSEMBLY_USAGE_OCCURRENCE ( 'NAUO7', ' ', ' ', #9279, #4799, $ ) ;
#15133 = NEXT_ASSEMBLY_USAGE_OCCURRENCE ( 'NAUO8', ' ', ' ', #9279, #7495, $ ) ;
#15134 = NEXT_ASSEMBLY_USAGE_OCCURRENCE ( 'NAUO9', ' ', ' ', #9279, #7495, $ ) ;
#15135 = NEXT_ASSEMBLY_USAGE_OCCURRENCE ( 'NAUO10', ' ', ' ', #9279, #7495, $ ) ;
#15136 = NEXT_ASSEMBLY_USAGE_OCCURRENCE ( 'NAUO11', ' ', ' ', #9279, #7495, $ ) ;
#15137 = NEXT_ASSEMBLY_USAGE_OCCURRENCE ( 'NAUO12', ' ', ' ', #9279, #7495, $ ) ;
ENDSEC;
END-ISO-10303-21;
